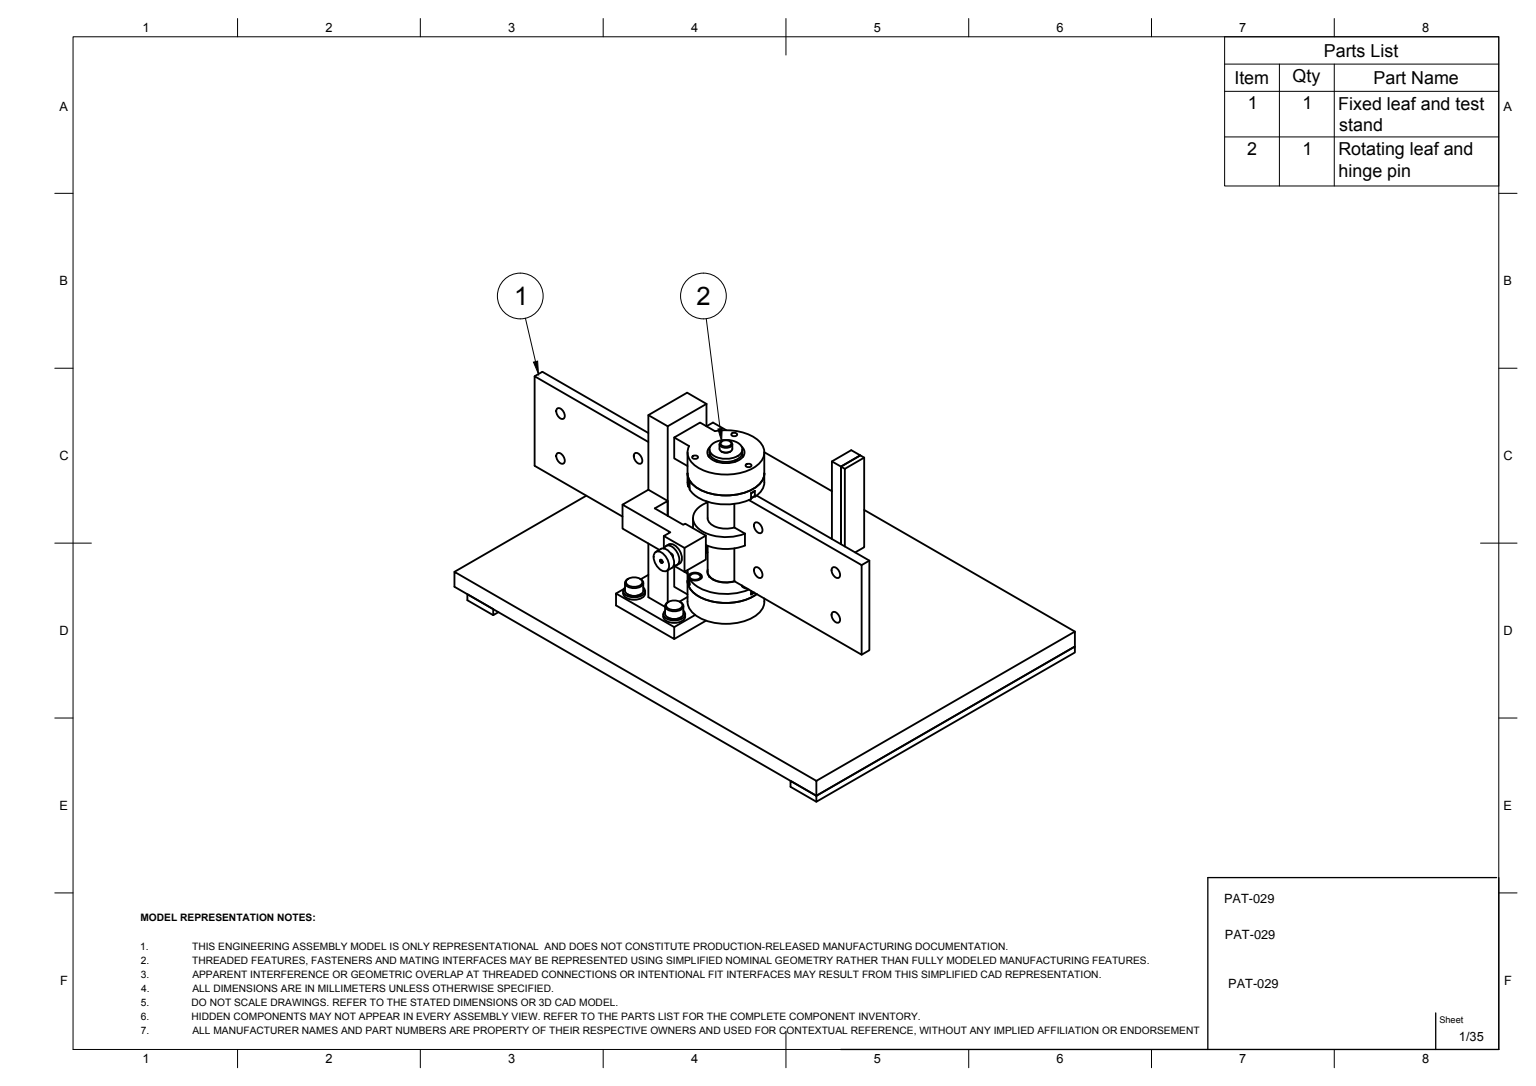
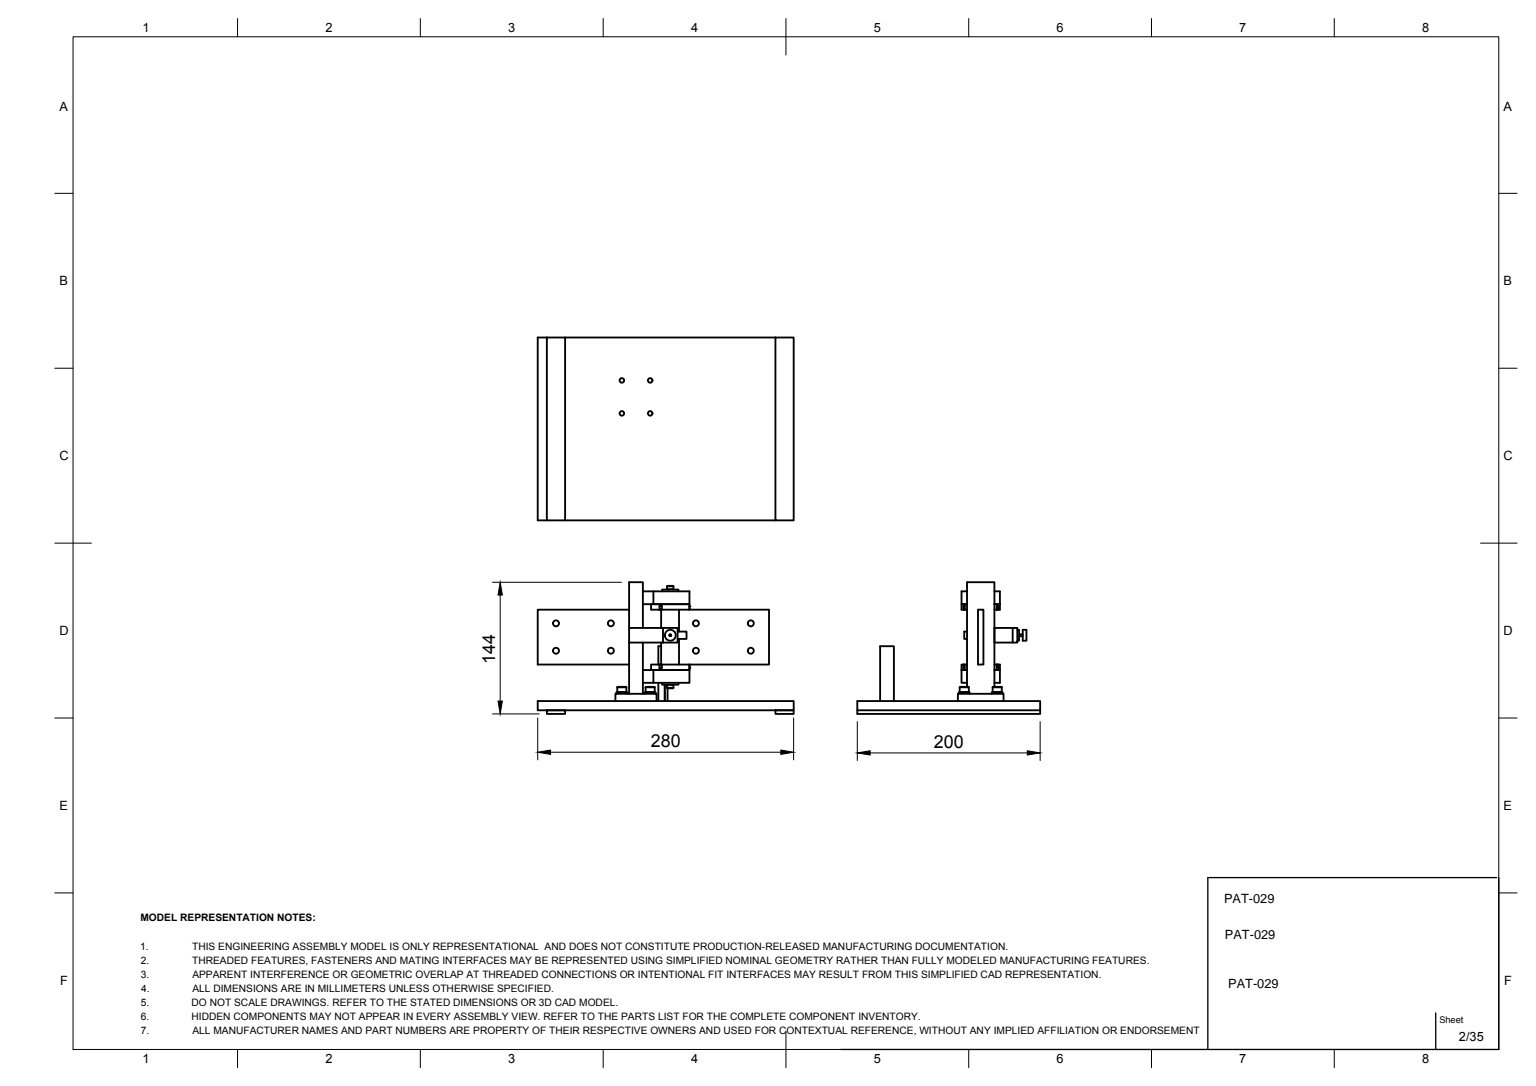
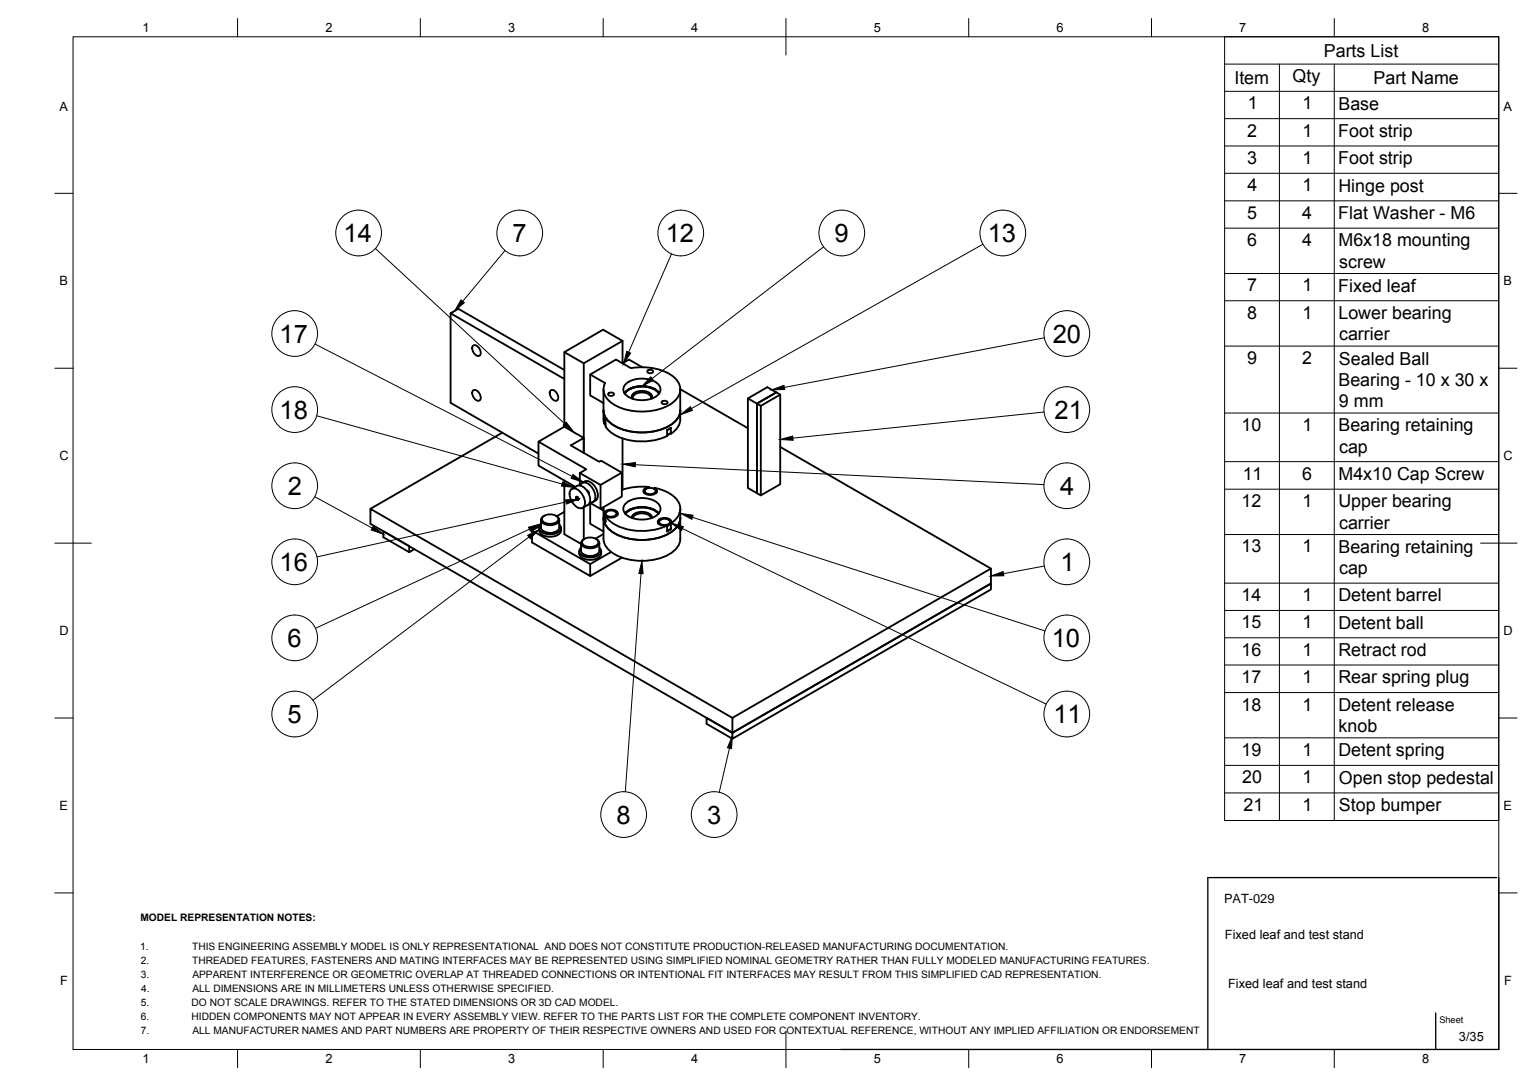
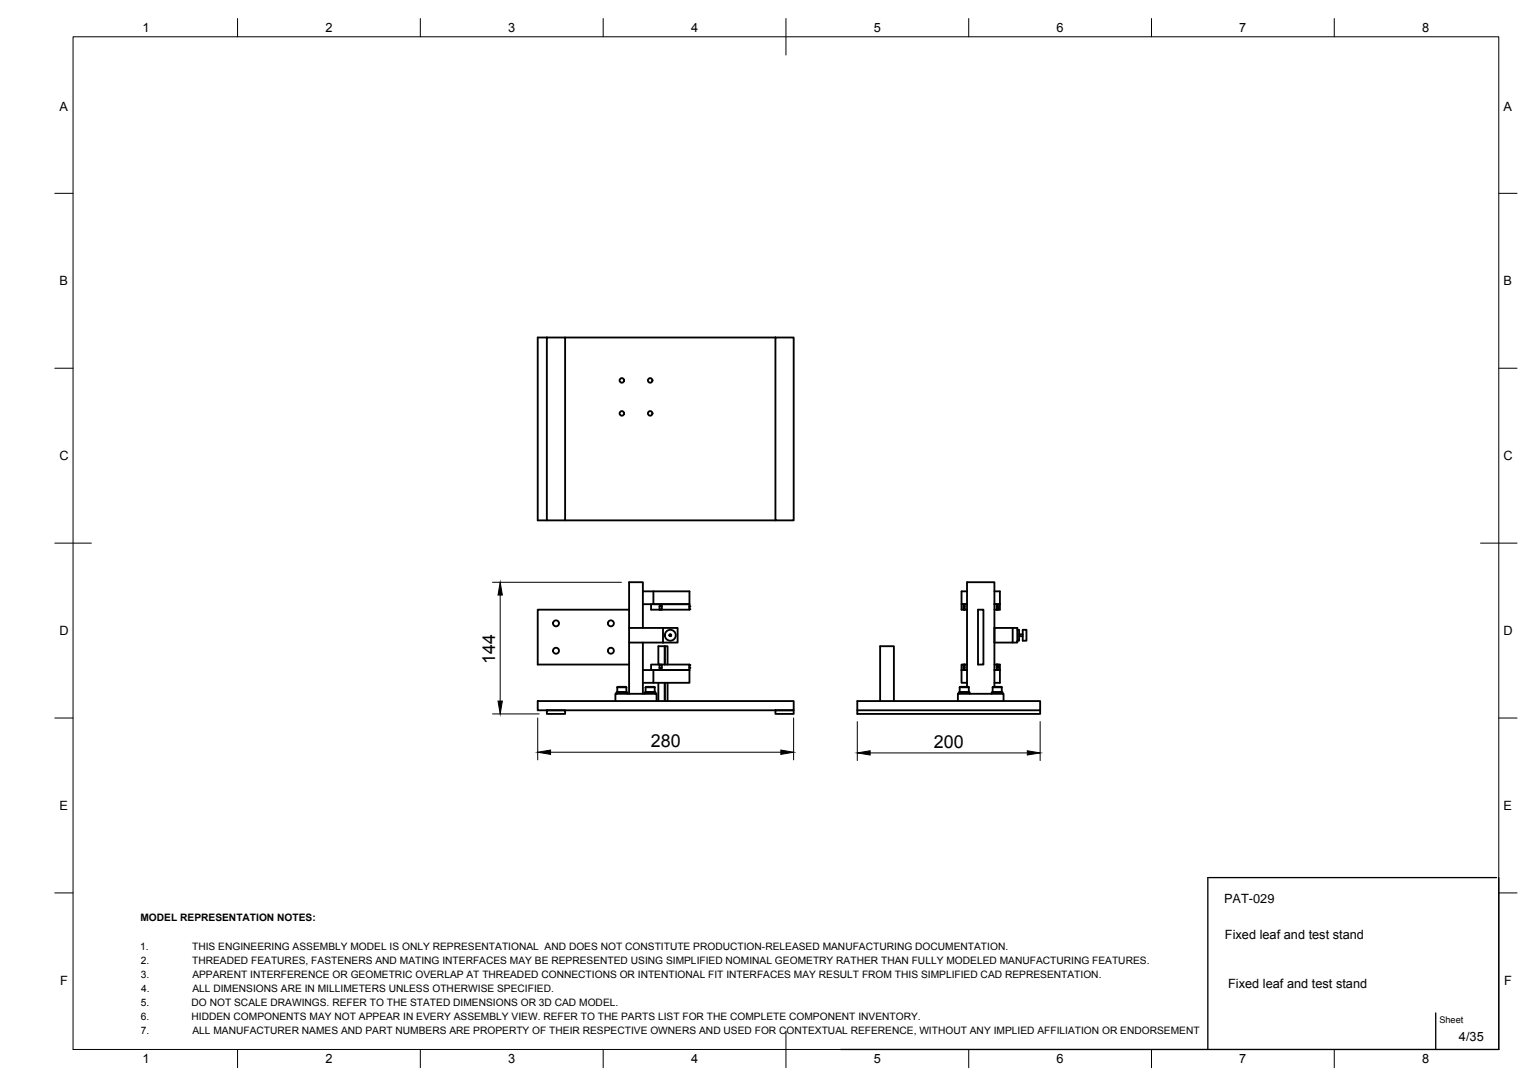
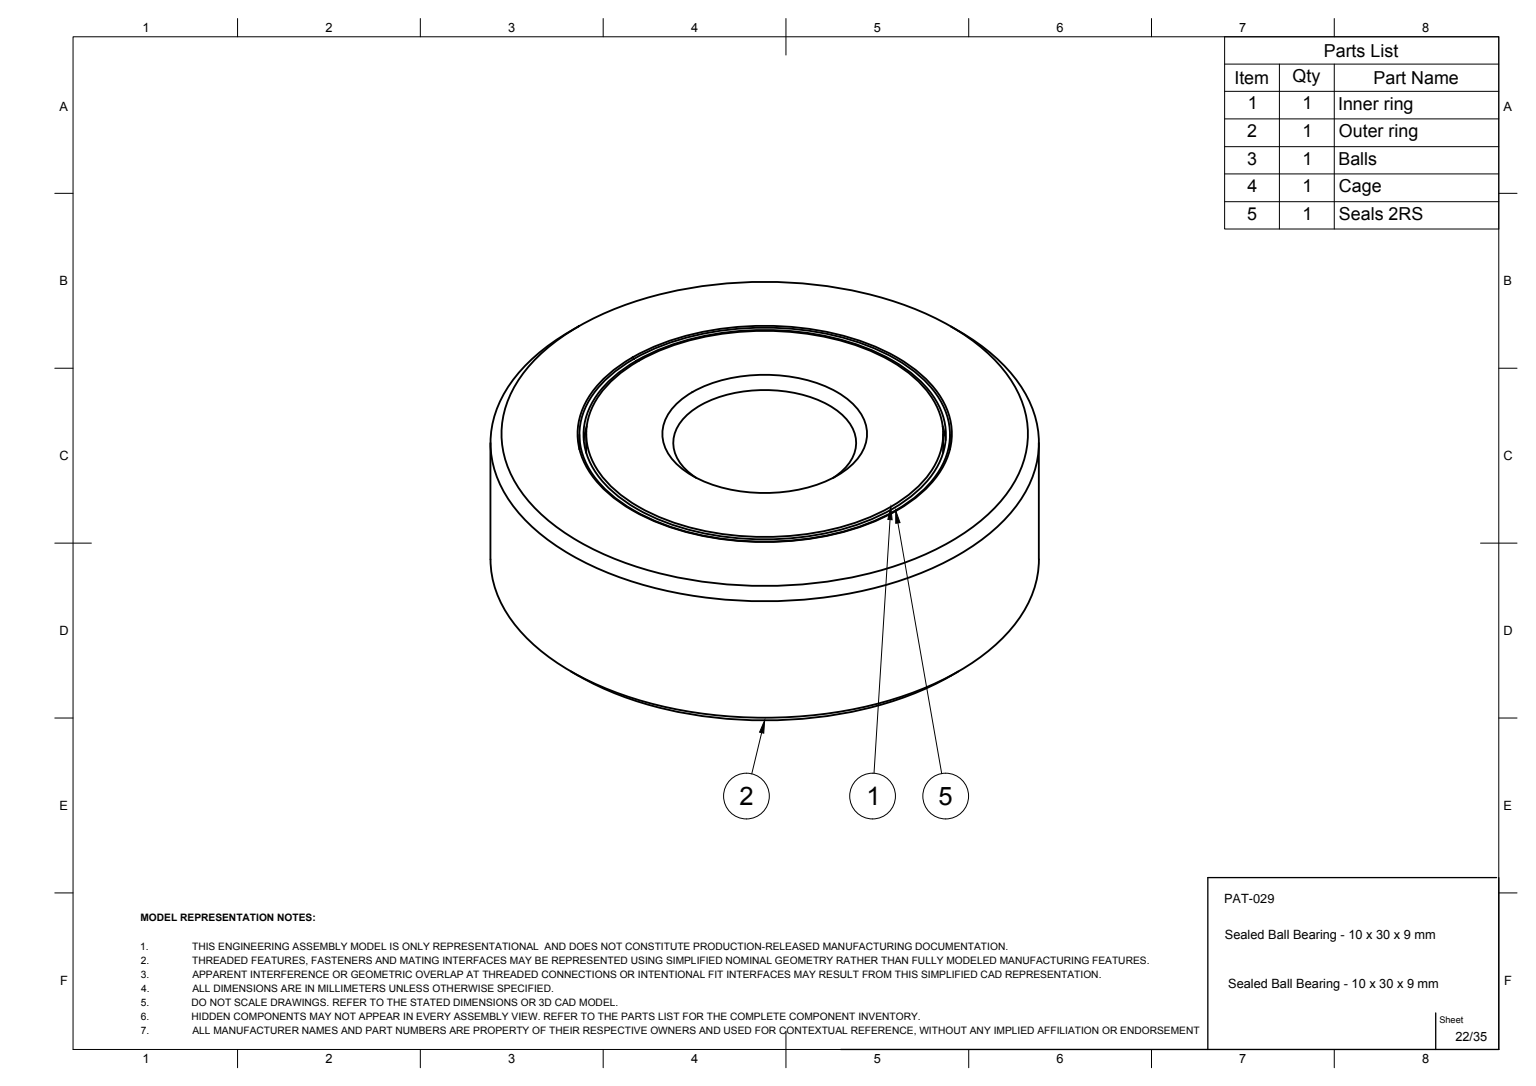
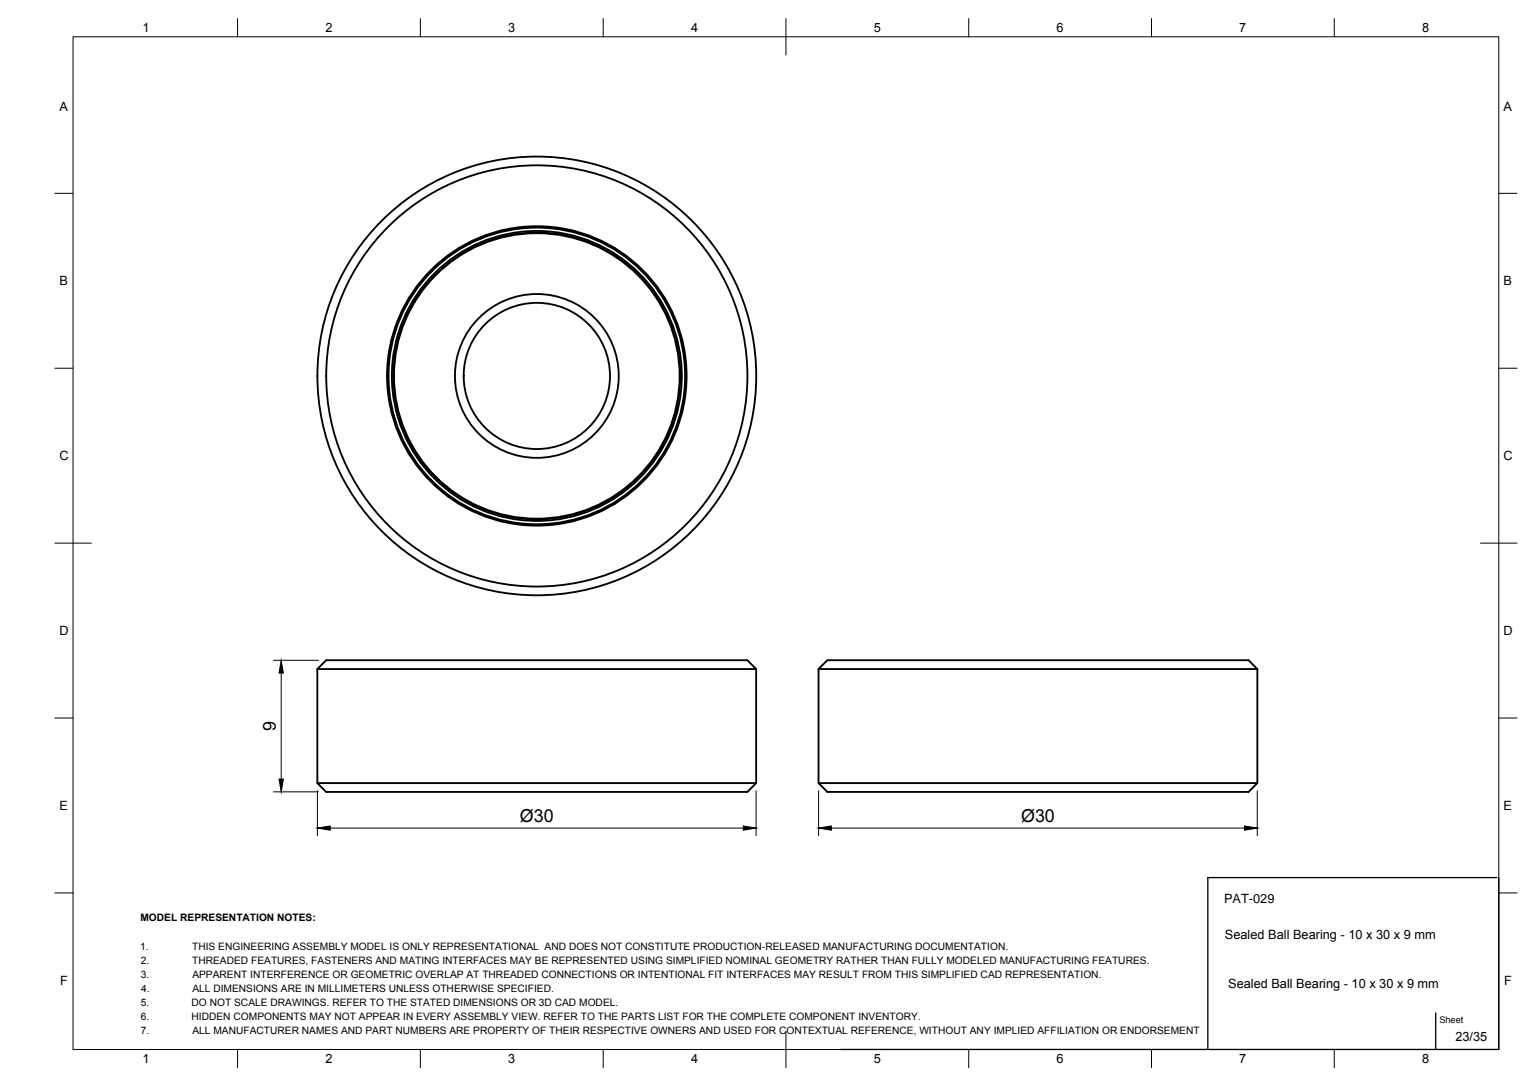
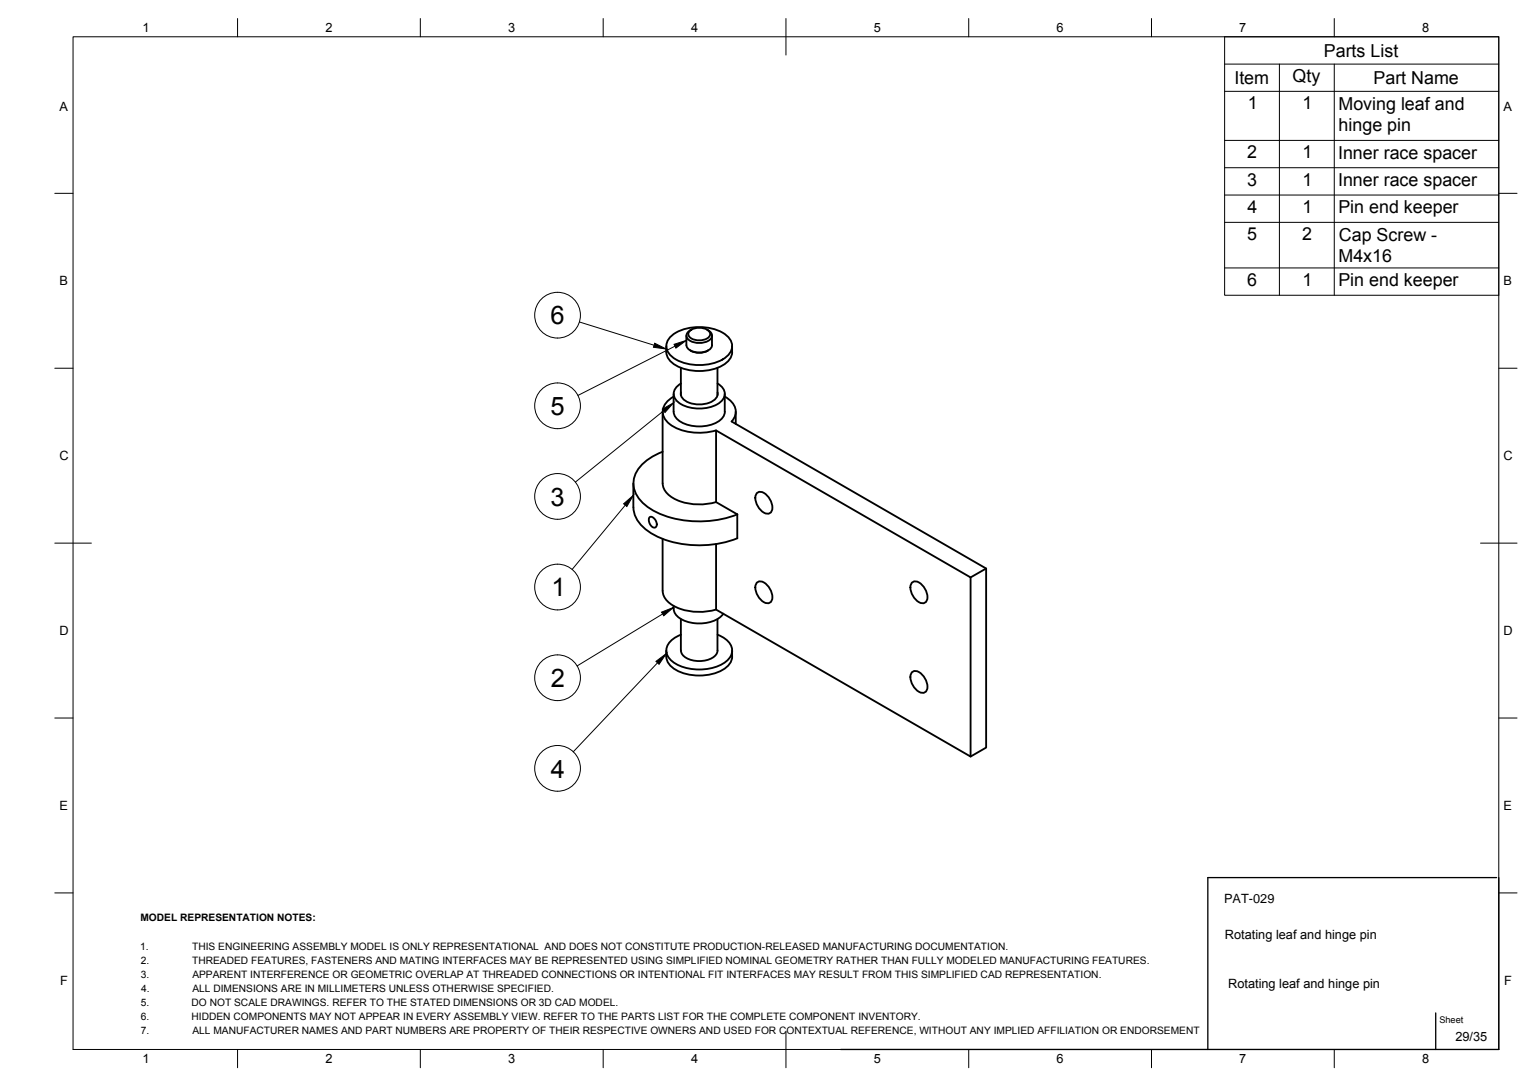
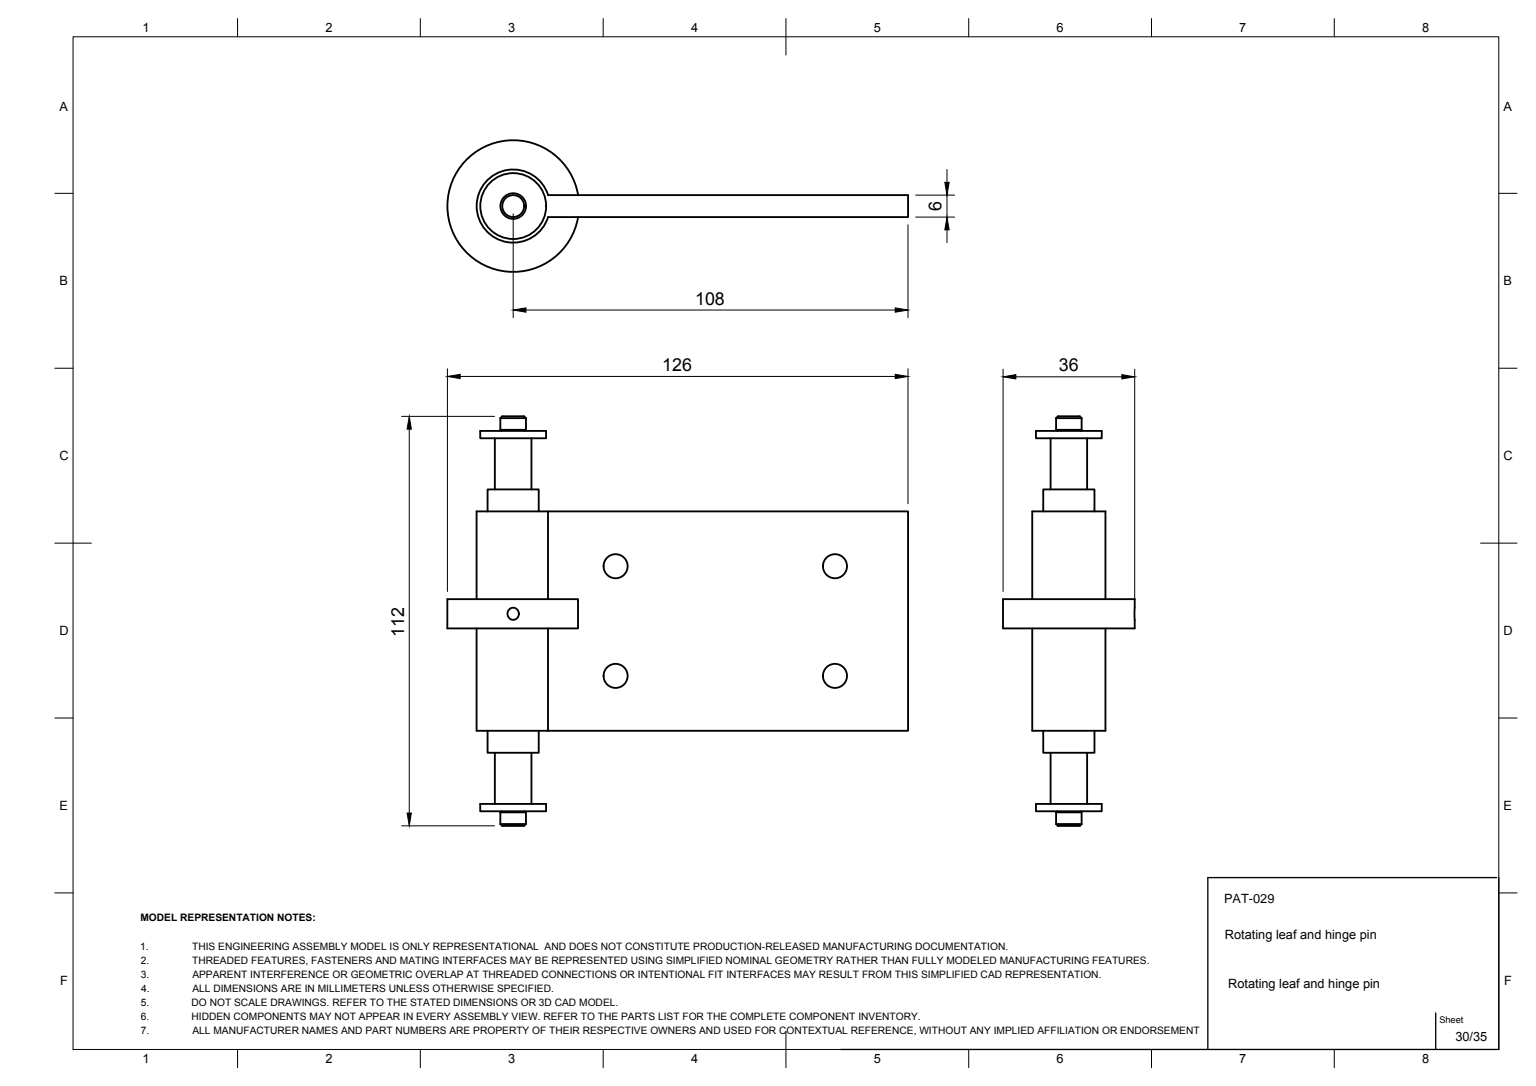
ISO-10303-21;
HEADER;
/* Generated by software containing ST-Developer
 * from STEP Tools, Inc. (www.steptools.com) 
 */

FILE_DESCRIPTION(
/* description */ ('Door-style hinge test fixture with detent'),
/* implementation_level */ '2;1');

FILE_NAME(
/* name */ 'PAT-029',
/* time_stamp */ '2026-10-28T03:24:57-07:00',
/* author */ (''),
/* organization */ (''),
/* preprocessor_version */ 'ST-DEVELOPER v20.2',
/* originating_system */ 'Autodesk Translation Framework v15.17.0.0',
/* authorisation */ '');

FILE_SCHEMA (('AUTOMOTIVE_DESIGN { 1 0 10303 214 3 1 1 }'));
ENDSEC;

DATA;
#10=MECHANICAL_DESIGN_GEOMETRIC_PRESENTATION_REPRESENTATION('',(#322,#323,
#324,#325,#326,#327,#328,#329,#330,#331,#332,#333,#334,#335,#336,#337,#338,
#339,#340,#341,#342,#343,#344,#345,#346,#347,#348,#349,#350,#351,#352,#353,
#354,#355,#356,#357,#358,#359,#360,#361),#9813);
#11=ITEM_DEFINED_TRANSFORMATION($,$,#5443,#5571);
#12=ITEM_DEFINED_TRANSFORMATION($,$,#5463,#5572);
#13=ITEM_DEFINED_TRANSFORMATION($,$,#5483,#5573);
#14=ITEM_DEFINED_TRANSFORMATION($,$,#5500,#5574);
#15=ITEM_DEFINED_TRANSFORMATION($,$,#5554,#5575);
#16=ITEM_DEFINED_TRANSFORMATION($,$,#5140,#5600);
#17=ITEM_DEFINED_TRANSFORMATION($,$,#5159,#5601);
#18=ITEM_DEFINED_TRANSFORMATION($,$,#5166,#5602);
#19=ITEM_DEFINED_TRANSFORMATION($,$,#5173,#5603);
#20=ITEM_DEFINED_TRANSFORMATION($,$,#5198,#5604);
#21=ITEM_DEFINED_TRANSFORMATION($,$,#5217,#5605);
#22=ITEM_DEFINED_TRANSFORMATION($,$,#5242,#5606);
#23=ITEM_DEFINED_TRANSFORMATION($,$,#5278,#5607);
#24=ITEM_DEFINED_TRANSFORMATION($,$,#5303,#5608);
#25=ITEM_DEFINED_TRANSFORMATION($,$,#5339,#5609);
#26=ITEM_DEFINED_TRANSFORMATION($,$,#5355,#5610);
#27=ITEM_DEFINED_TRANSFORMATION($,$,#5358,#5611);
#28=ITEM_DEFINED_TRANSFORMATION($,$,#5368,#5612);
#29=ITEM_DEFINED_TRANSFORMATION($,$,#5381,#5613);
#30=ITEM_DEFINED_TRANSFORMATION($,$,#5390,#5614);
#31=ITEM_DEFINED_TRANSFORMATION($,$,#5395,#5615);
#32=ITEM_DEFINED_TRANSFORMATION($,$,#5402,#5616);
#33=ITEM_DEFINED_TRANSFORMATION($,$,#5409,#5617);
#34=ITEM_DEFINED_TRANSFORMATION($,$,#5418,#5618);
#35=ITEM_DEFINED_TRANSFORMATION($,$,#5409,#5619);
#36=ITEM_DEFINED_TRANSFORMATION($,$,#5418,#5620);
#37=ITEM_DEFINED_TRANSFORMATION($,$,#5409,#5621);
#38=ITEM_DEFINED_TRANSFORMATION($,$,#5418,#5622);
#39=ITEM_DEFINED_TRANSFORMATION($,$,#5409,#5623);
#40=ITEM_DEFINED_TRANSFORMATION($,$,#5418,#5624);
#41=ITEM_DEFINED_TRANSFORMATION($,$,#5442,#5625);
#42=ITEM_DEFINED_TRANSFORMATION($,$,#5576,#5626);
#43=ITEM_DEFINED_TRANSFORMATION($,$,#5576,#5627);
#44=ITEM_DEFINED_TRANSFORMATION($,$,#5576,#5628);
#45=ITEM_DEFINED_TRANSFORMATION($,$,#5442,#5629);
#46=ITEM_DEFINED_TRANSFORMATION($,$,#5576,#5630);
#47=ITEM_DEFINED_TRANSFORMATION($,$,#5576,#5631);
#48=ITEM_DEFINED_TRANSFORMATION($,$,#5576,#5632);
#49=ITEM_DEFINED_TRANSFORMATION($,$,#5634,#5742);
#50=ITEM_DEFINED_TRANSFORMATION($,$,#5680,#5743);
#51=ITEM_DEFINED_TRANSFORMATION($,$,#5689,#5744);
#52=ITEM_DEFINED_TRANSFORMATION($,$,#5698,#5745);
#53=ITEM_DEFINED_TRANSFORMATION($,$,#5707,#5746);
#54=ITEM_DEFINED_TRANSFORMATION($,$,#5716,#5747);
#55=ITEM_DEFINED_TRANSFORMATION($,$,#5716,#5748);
#56=ITEM_DEFINED_TRANSFORMATION($,$,#5139,#5749);
#57=ITEM_DEFINED_TRANSFORMATION($,$,#5633,#5750);
#58=(
REPRESENTATION_RELATIONSHIP($,$,#9957,#9956)
REPRESENTATION_RELATIONSHIP_WITH_TRANSFORMATION(#11)
SHAPE_REPRESENTATION_RELATIONSHIP()
);
#59=(
REPRESENTATION_RELATIONSHIP($,$,#9958,#9956)
REPRESENTATION_RELATIONSHIP_WITH_TRANSFORMATION(#12)
SHAPE_REPRESENTATION_RELATIONSHIP()
);
#60=(
REPRESENTATION_RELATIONSHIP($,$,#9959,#9956)
REPRESENTATION_RELATIONSHIP_WITH_TRANSFORMATION(#13)
SHAPE_REPRESENTATION_RELATIONSHIP()
);
#61=(
REPRESENTATION_RELATIONSHIP($,$,#9960,#9956)
REPRESENTATION_RELATIONSHIP_WITH_TRANSFORMATION(#14)
SHAPE_REPRESENTATION_RELATIONSHIP()
);
#62=(
REPRESENTATION_RELATIONSHIP($,$,#9961,#9956)
REPRESENTATION_RELATIONSHIP_WITH_TRANSFORMATION(#15)
SHAPE_REPRESENTATION_RELATIONSHIP()
);
#63=(
REPRESENTATION_RELATIONSHIP($,$,#9937,#9936)
REPRESENTATION_RELATIONSHIP_WITH_TRANSFORMATION(#16)
SHAPE_REPRESENTATION_RELATIONSHIP()
);
#64=(
REPRESENTATION_RELATIONSHIP($,$,#9938,#9936)
REPRESENTATION_RELATIONSHIP_WITH_TRANSFORMATION(#17)
SHAPE_REPRESENTATION_RELATIONSHIP()
);
#65=(
REPRESENTATION_RELATIONSHIP($,$,#9939,#9936)
REPRESENTATION_RELATIONSHIP_WITH_TRANSFORMATION(#18)
SHAPE_REPRESENTATION_RELATIONSHIP()
);
#66=(
REPRESENTATION_RELATIONSHIP($,$,#9940,#9936)
REPRESENTATION_RELATIONSHIP_WITH_TRANSFORMATION(#19)
SHAPE_REPRESENTATION_RELATIONSHIP()
);
#67=(
REPRESENTATION_RELATIONSHIP($,$,#9941,#9936)
REPRESENTATION_RELATIONSHIP_WITH_TRANSFORMATION(#20)
SHAPE_REPRESENTATION_RELATIONSHIP()
);
#68=(
REPRESENTATION_RELATIONSHIP($,$,#9942,#9936)
REPRESENTATION_RELATIONSHIP_WITH_TRANSFORMATION(#21)
SHAPE_REPRESENTATION_RELATIONSHIP()
);
#69=(
REPRESENTATION_RELATIONSHIP($,$,#9943,#9936)
REPRESENTATION_RELATIONSHIP_WITH_TRANSFORMATION(#22)
SHAPE_REPRESENTATION_RELATIONSHIP()
);
#70=(
REPRESENTATION_RELATIONSHIP($,$,#9944,#9936)
REPRESENTATION_RELATIONSHIP_WITH_TRANSFORMATION(#23)
SHAPE_REPRESENTATION_RELATIONSHIP()
);
#71=(
REPRESENTATION_RELATIONSHIP($,$,#9945,#9936)
REPRESENTATION_RELATIONSHIP_WITH_TRANSFORMATION(#24)
SHAPE_REPRESENTATION_RELATIONSHIP()
);
#72=(
REPRESENTATION_RELATIONSHIP($,$,#9946,#9936)
REPRESENTATION_RELATIONSHIP_WITH_TRANSFORMATION(#25)
SHAPE_REPRESENTATION_RELATIONSHIP()
);
#73=(
REPRESENTATION_RELATIONSHIP($,$,#9947,#9936)
REPRESENTATION_RELATIONSHIP_WITH_TRANSFORMATION(#26)
SHAPE_REPRESENTATION_RELATIONSHIP()
);
#74=(
REPRESENTATION_RELATIONSHIP($,$,#9948,#9936)
REPRESENTATION_RELATIONSHIP_WITH_TRANSFORMATION(#27)
SHAPE_REPRESENTATION_RELATIONSHIP()
);
#75=(
REPRESENTATION_RELATIONSHIP($,$,#9949,#9936)
REPRESENTATION_RELATIONSHIP_WITH_TRANSFORMATION(#28)
SHAPE_REPRESENTATION_RELATIONSHIP()
);
#76=(
REPRESENTATION_RELATIONSHIP($,$,#9950,#9936)
REPRESENTATION_RELATIONSHIP_WITH_TRANSFORMATION(#29)
SHAPE_REPRESENTATION_RELATIONSHIP()
);
#77=(
REPRESENTATION_RELATIONSHIP($,$,#9951,#9936)
REPRESENTATION_RELATIONSHIP_WITH_TRANSFORMATION(#30)
SHAPE_REPRESENTATION_RELATIONSHIP()
);
#78=(
REPRESENTATION_RELATIONSHIP($,$,#9952,#9936)
REPRESENTATION_RELATIONSHIP_WITH_TRANSFORMATION(#31)
SHAPE_REPRESENTATION_RELATIONSHIP()
);
#79=(
REPRESENTATION_RELATIONSHIP($,$,#9953,#9936)
REPRESENTATION_RELATIONSHIP_WITH_TRANSFORMATION(#32)
SHAPE_REPRESENTATION_RELATIONSHIP()
);
#80=(
REPRESENTATION_RELATIONSHIP($,$,#9954,#9936)
REPRESENTATION_RELATIONSHIP_WITH_TRANSFORMATION(#33)
SHAPE_REPRESENTATION_RELATIONSHIP()
);
#81=(
REPRESENTATION_RELATIONSHIP($,$,#9955,#9936)
REPRESENTATION_RELATIONSHIP_WITH_TRANSFORMATION(#34)
SHAPE_REPRESENTATION_RELATIONSHIP()
);
#82=(
REPRESENTATION_RELATIONSHIP($,$,#9954,#9936)
REPRESENTATION_RELATIONSHIP_WITH_TRANSFORMATION(#35)
SHAPE_REPRESENTATION_RELATIONSHIP()
);
#83=(
REPRESENTATION_RELATIONSHIP($,$,#9955,#9936)
REPRESENTATION_RELATIONSHIP_WITH_TRANSFORMATION(#36)
SHAPE_REPRESENTATION_RELATIONSHIP()
);
#84=(
REPRESENTATION_RELATIONSHIP($,$,#9954,#9936)
REPRESENTATION_RELATIONSHIP_WITH_TRANSFORMATION(#37)
SHAPE_REPRESENTATION_RELATIONSHIP()
);
#85=(
REPRESENTATION_RELATIONSHIP($,$,#9955,#9936)
REPRESENTATION_RELATIONSHIP_WITH_TRANSFORMATION(#38)
SHAPE_REPRESENTATION_RELATIONSHIP()
);
#86=(
REPRESENTATION_RELATIONSHIP($,$,#9954,#9936)
REPRESENTATION_RELATIONSHIP_WITH_TRANSFORMATION(#39)
SHAPE_REPRESENTATION_RELATIONSHIP()
);
#87=(
REPRESENTATION_RELATIONSHIP($,$,#9955,#9936)
REPRESENTATION_RELATIONSHIP_WITH_TRANSFORMATION(#40)
SHAPE_REPRESENTATION_RELATIONSHIP()
);
#88=(
REPRESENTATION_RELATIONSHIP($,$,#9956,#9936)
REPRESENTATION_RELATIONSHIP_WITH_TRANSFORMATION(#41)
SHAPE_REPRESENTATION_RELATIONSHIP()
);
#89=(
REPRESENTATION_RELATIONSHIP($,$,#9962,#9936)
REPRESENTATION_RELATIONSHIP_WITH_TRANSFORMATION(#42)
SHAPE_REPRESENTATION_RELATIONSHIP()
);
#90=(
REPRESENTATION_RELATIONSHIP($,$,#9962,#9936)
REPRESENTATION_RELATIONSHIP_WITH_TRANSFORMATION(#43)
SHAPE_REPRESENTATION_RELATIONSHIP()
);
#91=(
REPRESENTATION_RELATIONSHIP($,$,#9962,#9936)
REPRESENTATION_RELATIONSHIP_WITH_TRANSFORMATION(#44)
SHAPE_REPRESENTATION_RELATIONSHIP()
);
#92=(
REPRESENTATION_RELATIONSHIP($,$,#9956,#9936)
REPRESENTATION_RELATIONSHIP_WITH_TRANSFORMATION(#45)
SHAPE_REPRESENTATION_RELATIONSHIP()
);
#93=(
REPRESENTATION_RELATIONSHIP($,$,#9962,#9936)
REPRESENTATION_RELATIONSHIP_WITH_TRANSFORMATION(#46)
SHAPE_REPRESENTATION_RELATIONSHIP()
);
#94=(
REPRESENTATION_RELATIONSHIP($,$,#9962,#9936)
REPRESENTATION_RELATIONSHIP_WITH_TRANSFORMATION(#47)
SHAPE_REPRESENTATION_RELATIONSHIP()
);
#95=(
REPRESENTATION_RELATIONSHIP($,$,#9962,#9936)
REPRESENTATION_RELATIONSHIP_WITH_TRANSFORMATION(#48)
SHAPE_REPRESENTATION_RELATIONSHIP()
);
#96=(
REPRESENTATION_RELATIONSHIP($,$,#9964,#9963)
REPRESENTATION_RELATIONSHIP_WITH_TRANSFORMATION(#49)
SHAPE_REPRESENTATION_RELATIONSHIP()
);
#97=(
REPRESENTATION_RELATIONSHIP($,$,#9965,#9963)
REPRESENTATION_RELATIONSHIP_WITH_TRANSFORMATION(#50)
SHAPE_REPRESENTATION_RELATIONSHIP()
);
#98=(
REPRESENTATION_RELATIONSHIP($,$,#9966,#9963)
REPRESENTATION_RELATIONSHIP_WITH_TRANSFORMATION(#51)
SHAPE_REPRESENTATION_RELATIONSHIP()
);
#99=(
REPRESENTATION_RELATIONSHIP($,$,#9967,#9963)
REPRESENTATION_RELATIONSHIP_WITH_TRANSFORMATION(#52)
SHAPE_REPRESENTATION_RELATIONSHIP()
);
#100=(
REPRESENTATION_RELATIONSHIP($,$,#9968,#9963)
REPRESENTATION_RELATIONSHIP_WITH_TRANSFORMATION(#53)
SHAPE_REPRESENTATION_RELATIONSHIP()
);
#101=(
REPRESENTATION_RELATIONSHIP($,$,#9969,#9963)
REPRESENTATION_RELATIONSHIP_WITH_TRANSFORMATION(#54)
SHAPE_REPRESENTATION_RELATIONSHIP()
);
#102=(
REPRESENTATION_RELATIONSHIP($,$,#9969,#9963)
REPRESENTATION_RELATIONSHIP_WITH_TRANSFORMATION(#55)
SHAPE_REPRESENTATION_RELATIONSHIP()
);
#103=(
REPRESENTATION_RELATIONSHIP($,$,#9936,#9935)
REPRESENTATION_RELATIONSHIP_WITH_TRANSFORMATION(#56)
SHAPE_REPRESENTATION_RELATIONSHIP()
);
#104=(
REPRESENTATION_RELATIONSHIP($,$,#9963,#9935)
REPRESENTATION_RELATIONSHIP_WITH_TRANSFORMATION(#57)
SHAPE_REPRESENTATION_RELATIONSHIP()
);
#105=CONTEXT_DEPENDENT_SHAPE_REPRESENTATION(#58,#9880);
#106=CONTEXT_DEPENDENT_SHAPE_REPRESENTATION(#59,#9881);
#107=CONTEXT_DEPENDENT_SHAPE_REPRESENTATION(#60,#9882);
#108=CONTEXT_DEPENDENT_SHAPE_REPRESENTATION(#61,#9883);
#109=CONTEXT_DEPENDENT_SHAPE_REPRESENTATION(#62,#9884);
#110=CONTEXT_DEPENDENT_SHAPE_REPRESENTATION(#63,#9886);
#111=CONTEXT_DEPENDENT_SHAPE_REPRESENTATION(#64,#9887);
#112=CONTEXT_DEPENDENT_SHAPE_REPRESENTATION(#65,#9888);
#113=CONTEXT_DEPENDENT_SHAPE_REPRESENTATION(#66,#9889);
#114=CONTEXT_DEPENDENT_SHAPE_REPRESENTATION(#67,#9890);
#115=CONTEXT_DEPENDENT_SHAPE_REPRESENTATION(#68,#9891);
#116=CONTEXT_DEPENDENT_SHAPE_REPRESENTATION(#69,#9892);
#117=CONTEXT_DEPENDENT_SHAPE_REPRESENTATION(#70,#9893);
#118=CONTEXT_DEPENDENT_SHAPE_REPRESENTATION(#71,#9894);
#119=CONTEXT_DEPENDENT_SHAPE_REPRESENTATION(#72,#9895);
#120=CONTEXT_DEPENDENT_SHAPE_REPRESENTATION(#73,#9896);
#121=CONTEXT_DEPENDENT_SHAPE_REPRESENTATION(#74,#9897);
#122=CONTEXT_DEPENDENT_SHAPE_REPRESENTATION(#75,#9898);
#123=CONTEXT_DEPENDENT_SHAPE_REPRESENTATION(#76,#9899);
#124=CONTEXT_DEPENDENT_SHAPE_REPRESENTATION(#77,#9900);
#125=CONTEXT_DEPENDENT_SHAPE_REPRESENTATION(#78,#9901);
#126=CONTEXT_DEPENDENT_SHAPE_REPRESENTATION(#79,#9902);
#127=CONTEXT_DEPENDENT_SHAPE_REPRESENTATION(#80,#9903);
#128=CONTEXT_DEPENDENT_SHAPE_REPRESENTATION(#81,#9904);
#129=CONTEXT_DEPENDENT_SHAPE_REPRESENTATION(#82,#9905);
#130=CONTEXT_DEPENDENT_SHAPE_REPRESENTATION(#83,#9906);
#131=CONTEXT_DEPENDENT_SHAPE_REPRESENTATION(#84,#9907);
#132=CONTEXT_DEPENDENT_SHAPE_REPRESENTATION(#85,#9908);
#133=CONTEXT_DEPENDENT_SHAPE_REPRESENTATION(#86,#9909);
#134=CONTEXT_DEPENDENT_SHAPE_REPRESENTATION(#87,#9910);
#135=CONTEXT_DEPENDENT_SHAPE_REPRESENTATION(#88,#9911);
#136=CONTEXT_DEPENDENT_SHAPE_REPRESENTATION(#89,#9912);
#137=CONTEXT_DEPENDENT_SHAPE_REPRESENTATION(#90,#9913);
#138=CONTEXT_DEPENDENT_SHAPE_REPRESENTATION(#91,#9914);
#139=CONTEXT_DEPENDENT_SHAPE_REPRESENTATION(#92,#9915);
#140=CONTEXT_DEPENDENT_SHAPE_REPRESENTATION(#93,#9916);
#141=CONTEXT_DEPENDENT_SHAPE_REPRESENTATION(#94,#9917);
#142=CONTEXT_DEPENDENT_SHAPE_REPRESENTATION(#95,#9918);
#143=CONTEXT_DEPENDENT_SHAPE_REPRESENTATION(#96,#9926);
#144=CONTEXT_DEPENDENT_SHAPE_REPRESENTATION(#97,#9927);
#145=CONTEXT_DEPENDENT_SHAPE_REPRESENTATION(#98,#9928);
#146=CONTEXT_DEPENDENT_SHAPE_REPRESENTATION(#99,#9929);
#147=CONTEXT_DEPENDENT_SHAPE_REPRESENTATION(#100,#9930);
#148=CONTEXT_DEPENDENT_SHAPE_REPRESENTATION(#101,#9931);
#149=CONTEXT_DEPENDENT_SHAPE_REPRESENTATION(#102,#9932);
#150=CONTEXT_DEPENDENT_SHAPE_REPRESENTATION(#103,#9933);
#151=CONTEXT_DEPENDENT_SHAPE_REPRESENTATION(#104,#9934);
#152=NEXT_ASSEMBLY_USAGE_OCCURRENCE('Inner ring:1','Inner ring:1',
'Inner ring:1',#9992,#9993,'Inner ring:1');
#153=NEXT_ASSEMBLY_USAGE_OCCURRENCE('Outer ring:1','Outer ring:1',
'Outer ring:1',#9992,#9994,'Outer ring:1');
#154=NEXT_ASSEMBLY_USAGE_OCCURRENCE('Balls:1','Balls:1','Balls:1',#9992,
#9995,'Balls:1');
#155=NEXT_ASSEMBLY_USAGE_OCCURRENCE('Cage:1','Cage:1','Cage:1',#9992,#9996,
'Cage:1');
#156=NEXT_ASSEMBLY_USAGE_OCCURRENCE('Seals 2RS:1','Seals 2RS:1',
'Seals 2RS:1',#9992,#9997,'Seals 2RS:1');
#157=NEXT_ASSEMBLY_USAGE_OCCURRENCE('Base:1','Base:1','Base:1',#9972,#9973,
'Base:1');
#158=NEXT_ASSEMBLY_USAGE_OCCURRENCE('Foot strip:1','Foot strip:1',
'Foot strip:1',#9972,#9974,'Foot strip:1');
#159=NEXT_ASSEMBLY_USAGE_OCCURRENCE('Foot strip (1):1',
'Foot strip (1):1','Foot strip (1):1',#9972,#9975,'Foot strip (1):1');
#160=NEXT_ASSEMBLY_USAGE_OCCURRENCE('Hinge post:1','Hinge post:1',
'Hinge post:1',#9972,#9976,'Hinge post:1');
#161=NEXT_ASSEMBLY_USAGE_OCCURRENCE('Fixed leaf:1','Fixed leaf:1',
'Fixed leaf:1',#9972,#9977,'Fixed leaf:1');
#162=NEXT_ASSEMBLY_USAGE_OCCURRENCE('Lower bearing carrier:1',
'Lower bearing carrier:1','Lower bearing carrier:1',#9972,#9978,
'Lower bearing carrier:1');
#163=NEXT_ASSEMBLY_USAGE_OCCURRENCE('Bearing retaining cap:1',
'Bearing retaining cap:1','Bearing retaining cap:1',#9972,#9979,
'Bearing retaining cap:1');
#164=NEXT_ASSEMBLY_USAGE_OCCURRENCE('Upper bearing carrier:1',
'Upper bearing carrier:1','Upper bearing carrier:1',#9972,#9980,
'Upper bearing carrier:1');
#165=NEXT_ASSEMBLY_USAGE_OCCURRENCE('Bearing retaining cap (1):1',
'Bearing retaining cap (1):1','Bearing retaining cap (1):1',#9972,#9981,
'Bearing retaining cap (1):1');
#166=NEXT_ASSEMBLY_USAGE_OCCURRENCE('Detent barrel:1','Detent barrel:1',
'Detent barrel:1',#9972,#9982,'Detent barrel:1');
#167=NEXT_ASSEMBLY_USAGE_OCCURRENCE('Detent ball:1','Detent ball:1',
'Detent ball:1',#9972,#9983,'Detent ball:1');
#168=NEXT_ASSEMBLY_USAGE_OCCURRENCE('Retract rod:1','Retract rod:1',
'Retract rod:1',#9972,#9984,'Retract rod:1');
#169=NEXT_ASSEMBLY_USAGE_OCCURRENCE('Rear spring plug:1',
'Rear spring plug:1','Rear spring plug:1',#9972,#9985,
'Rear spring plug:1');
#170=NEXT_ASSEMBLY_USAGE_OCCURRENCE('Detent release knob:1',
'Detent release knob:1','Detent release knob:1',#9972,#9986,
'Detent release knob:1');
#171=NEXT_ASSEMBLY_USAGE_OCCURRENCE('Detent spring:1','Detent spring:1',
'Detent spring:1',#9972,#9987,'Detent spring:1');
#172=NEXT_ASSEMBLY_USAGE_OCCURRENCE('Open stop pedestal:1',
'Open stop pedestal:1','Open stop pedestal:1',#9972,#9988,
'Open stop pedestal:1');
#173=NEXT_ASSEMBLY_USAGE_OCCURRENCE('Stop bumper:1','Stop bumper:1',
'Stop bumper:1',#9972,#9989,'Stop bumper:1');
#174=NEXT_ASSEMBLY_USAGE_OCCURRENCE('Flat Washer - M6:2',
'Flat Washer - M6:2','Flat Washer - M6:2',#9972,#9990,
'Flat Washer - M6:2');
#175=NEXT_ASSEMBLY_USAGE_OCCURRENCE('M6x18 mounting screw:2',
'M6x18 mounting screw:2','M6x18 mounting screw:2',#9972,#9991,
'M6x18 mounting screw:2');
#176=NEXT_ASSEMBLY_USAGE_OCCURRENCE('Flat Washer - M6:3',
'Flat Washer - M6:3','Flat Washer - M6:3',#9972,#9990,
'Flat Washer - M6:3');
#177=NEXT_ASSEMBLY_USAGE_OCCURRENCE('M6x18 mounting screw:3',
'M6x18 mounting screw:3','M6x18 mounting screw:3',#9972,#9991,
'M6x18 mounting screw:3');
#178=NEXT_ASSEMBLY_USAGE_OCCURRENCE('Flat Washer - M6:4',
'Flat Washer - M6:4','Flat Washer - M6:4',#9972,#9990,
'Flat Washer - M6:4');
#179=NEXT_ASSEMBLY_USAGE_OCCURRENCE('M6x18 mounting screw:4',
'M6x18 mounting screw:4','M6x18 mounting screw:4',#9972,#9991,
'M6x18 mounting screw:4');
#180=NEXT_ASSEMBLY_USAGE_OCCURRENCE('Flat Washer - M6:5',
'Flat Washer - M6:5','Flat Washer - M6:5',#9972,#9990,
'Flat Washer - M6:5');
#181=NEXT_ASSEMBLY_USAGE_OCCURRENCE('M6x18 mounting screw:5',
'M6x18 mounting screw:5','M6x18 mounting screw:5',#9972,#9991,
'M6x18 mounting screw:5');
#182=NEXT_ASSEMBLY_USAGE_OCCURRENCE(
'Sealed Ball Bearing - 10 x 30 x 9 mm:2',
'Sealed Ball Bearing - 10 x 30 x 9 mm:2',
'Sealed Ball Bearing - 10 x 30 x 9 mm:2',#9972,#9992,
'Sealed Ball Bearing - 10 x 30 x 9 mm:2');
#183=NEXT_ASSEMBLY_USAGE_OCCURRENCE('M4x10 Cap Screw:2',
'M4x10 Cap Screw:2','M4x10 Cap Screw:2',#9972,#9998,'M4x10 Cap Screw:2');
#184=NEXT_ASSEMBLY_USAGE_OCCURRENCE('M4x10 Cap Screw:3',
'M4x10 Cap Screw:3','M4x10 Cap Screw:3',#9972,#9998,'M4x10 Cap Screw:3');
#185=NEXT_ASSEMBLY_USAGE_OCCURRENCE('M4x10 Cap Screw:4',
'M4x10 Cap Screw:4','M4x10 Cap Screw:4',#9972,#9998,'M4x10 Cap Screw:4');
#186=NEXT_ASSEMBLY_USAGE_OCCURRENCE(
'Sealed Ball Bearing - 10 x 30 x 9 mm:3',
'Sealed Ball Bearing - 10 x 30 x 9 mm:3',
'Sealed Ball Bearing - 10 x 30 x 9 mm:3',#9972,#9992,
'Sealed Ball Bearing - 10 x 30 x 9 mm:3');
#187=NEXT_ASSEMBLY_USAGE_OCCURRENCE('M4x10 Cap Screw:5',
'M4x10 Cap Screw:5','M4x10 Cap Screw:5',#9972,#9998,'M4x10 Cap Screw:5');
#188=NEXT_ASSEMBLY_USAGE_OCCURRENCE('M4x10 Cap Screw:6',
'M4x10 Cap Screw:6','M4x10 Cap Screw:6',#9972,#9998,'M4x10 Cap Screw:6');
#189=NEXT_ASSEMBLY_USAGE_OCCURRENCE('M4x10 Cap Screw:7',
'M4x10 Cap Screw:7','M4x10 Cap Screw:7',#9972,#9998,'M4x10 Cap Screw:7');
#190=NEXT_ASSEMBLY_USAGE_OCCURRENCE('Moving leaf and hinge pin:1',
'Moving leaf and hinge pin:1','Moving leaf and hinge pin:1',#9999,#10000,
'Moving leaf and hinge pin:1');
#191=NEXT_ASSEMBLY_USAGE_OCCURRENCE('Inner race spacer:1',
'Inner race spacer:1','Inner race spacer:1',#9999,#10001,
'Inner race spacer:1');
#192=NEXT_ASSEMBLY_USAGE_OCCURRENCE('Inner race spacer (1):1',
'Inner race spacer (1):1','Inner race spacer (1):1',#9999,#10002,
'Inner race spacer (1):1');
#193=NEXT_ASSEMBLY_USAGE_OCCURRENCE('Pin end keeper:1',
'Pin end keeper:1','Pin end keeper:1',#9999,#10003,'Pin end keeper:1');
#194=NEXT_ASSEMBLY_USAGE_OCCURRENCE('Pin end keeper (1):1',
'Pin end keeper (1):1','Pin end keeper (1):1',#9999,#10004,
'Pin end keeper (1):1');
#195=NEXT_ASSEMBLY_USAGE_OCCURRENCE('Cap Screw - M4x16:2',
'Cap Screw - M4x16:2','Cap Screw - M4x16:2',#9999,#10005,
'Cap Screw - M4x16:2');
#196=NEXT_ASSEMBLY_USAGE_OCCURRENCE('Cap Screw - M4x16:3',
'Cap Screw - M4x16:3','Cap Screw - M4x16:3',#9999,#10005,
'Cap Screw - M4x16:3');
#197=NEXT_ASSEMBLY_USAGE_OCCURRENCE('Fixed leaf and test stand:1',
'Fixed leaf and test stand:1','Fixed leaf and test stand:1',#9971,#9972,
'Fixed leaf and test stand:1');
#198=NEXT_ASSEMBLY_USAGE_OCCURRENCE('Rotating leaf and hinge pin:1',
'Rotating leaf and hinge pin:1','Rotating leaf and hinge pin:1',#9971,#9999,
'Rotating leaf and hinge pin:1');
#199=TOROIDAL_SURFACE('',#5444,1.,0.247676);
#200=TOROIDAL_SURFACE('',#5464,1.,0.247676);
#201=CONICAL_SURFACE('',#5431,0.475,0.785398163397449);
#202=CONICAL_SURFACE('',#5435,0.485,0.785398163397448);
#203=CONICAL_SURFACE('',#5439,0.31,0.463647609000806);
#204=CONICAL_SURFACE('',#5455,0.53,0.785398163397448);
#205=CONICAL_SURFACE('',#5462,0.53,0.785398163397448);
#206=CONICAL_SURFACE('',#5475,1.47,0.785398163397449);
#207=CONICAL_SURFACE('',#5479,1.47,0.785398163397449);
#208=CONICAL_SURFACE('',#5589,0.325,0.785398163397448);
#209=CONICAL_SURFACE('',#5593,0.335,0.785398163397448);
#210=CONICAL_SURFACE('',#5597,0.21,0.463647609000806);
#211=CONICAL_SURFACE('',#5719,0.325,0.785398163397448);
#212=CONICAL_SURFACE('',#5723,0.335,0.785398163397448);
#213=CONICAL_SURFACE('',#5727,0.21,0.463647609000806);
#214=CONICAL_SURFACE('',#5731,0.18,0.785398163397448);
#215=ORIENTED_CLOSED_SHELL('',*,#4772,.F.);
#216=ORIENTED_CLOSED_SHELL('',*,#4787,.F.);
#217=ORIENTED_CLOSED_SHELL('',*,#4795,.F.);
#218=BREP_WITH_VOIDS('Body1',#4773,(#215));
#219=BREP_WITH_VOIDS('Body1',#4788,(#216));
#220=BREP_WITH_VOIDS('Body1',#4794,(#217));
#221=B_SPLINE_CURVE_WITH_KNOTS('',3,(#8567,#8568,#8569,#8570,#8571,#8572,
#8573,#8574,#8575,#8576,#8577,#8578,#8579,#8580,#8581,#8582,#8583,#8584,
#8585,#8586,#8587,#8588,#8589,#8590,#8591,#8592,#8593,#8594,#8595,#8596,
#8597,#8598,#8599,#8600,#8601,#8602,#8603,#8604,#8605,#8606,#8607,#8608,
#8609,#8610,#8611,#8612,#8613,#8614,#8615,#8616,#8617,#8618,#8619,#8620,
#8621,#8622,#8623,#8624,#8625,#8626,#8627,#8628,#8629,#8630,#8631),
 .UNSPECIFIED.,.F.,.F.,(4,1,1,1,1,1,1,1,1,1,1,1,1,1,1,1,1,1,1,1,1,1,1,1,
1,1,1,1,1,1,1,1,1,1,1,1,1,1,1,1,1,1,1,1,1,1,1,1,1,1,1,1,1,1,1,1,1,1,1,1,
1,1,4),(0.,0.0178571428571429,0.0357142857142857,0.0535714285714286,0.0714285714285714,
0.0892857142857143,0.107142857142857,0.125,0.142857142857143,0.158730158730159,
0.174603174603175,0.19047619047619,0.202380952380952,0.214285714285714,
0.226190476190476,0.238095238095238,0.25,0.261904761904762,0.273809523809524,
0.285714285714286,0.30952380952381,0.333333333333333,0.357142857142857,
0.380952380952381,0.404761904761905,0.428571428571429,0.446428571428571,
0.464285714285714,0.482142857142857,0.5,0.508928571428571,0.517857142857143,
0.535714285714286,0.553571428571429,0.571428571428571,0.589285714285714,
0.607142857142857,0.625,0.642857142857143,0.660714285714286,0.678571428571428,
0.696428571428571,0.714285714285714,0.738095238095238,0.75,0.761904761904762,
0.773809523809524,0.785714285714286,0.797619047619047,0.809523809523809,
0.821428571428571,0.833333333333333,0.845238095238095,0.857142857142857,
0.866071428571429,0.875,0.892857142857143,0.910714285714286,0.928571428571429,
0.946428571428571,0.964285714285714,0.982142857142857,1.),.UNSPECIFIED.);
#222=B_SPLINE_CURVE_WITH_KNOTS('',3,(#8878,#8879,#8880,#8881,#8882,#8883,
#8884,#8885,#8886,#8887,#8888,#8889,#8890,#8891,#8892,#8893,#8894,#8895,
#8896,#8897,#8898,#8899),.UNSPECIFIED.,.F.,.F.,(4,2,2,2,2,2,2,2,2,2,4),
(0.0473477652366656,0.126350602536658,0.189525903804987,0.252701205073317,
0.313298422430275,0.373895639787233,0.434492857144191,0.495090074501149,
0.558265375769478,0.621440677037807,0.7004435143378),.UNSPECIFIED.);
#223=B_SPLINE_CURVE_WITH_KNOTS('',3,(#8903,#8904,#8905,#8906,#8907,#8908,
#8909,#8910,#8911,#8912,#8913,#8914,#8915,#8916,#8917,#8918,#8919,#8920,
#8921,#8922,#8923,#8924),.UNSPECIFIED.,.F.,.F.,(4,2,2,2,2,2,2,2,2,2,4),
(0.0464897534940957,0.0852567806515119,0.170513561303024,0.246687263103517,
0.308657850341199,0.370628437578881,0.432599024816563,0.494569612054245,
0.570743313854739,0.656000094506251,0.694767121663666),.UNSPECIFIED.);
#224=B_SPLINE_CURVE_WITH_KNOTS('',3,(#8930,#8931,#8932,#8933,#8934,#8935,
#8936,#8937,#8938,#8939,#8940,#8941,#8942,#8943,#8944,#8945,#8946,#8947,
#8948,#8949,#8950,#8951),.UNSPECIFIED.,.F.,.F.,(4,2,2,2,2,2,2,2,2,2,4),
(0.0464897534940957,0.0852567806515118,0.170513561303024,0.246687263103517,
0.308657850341199,0.370628437578881,0.432599024816563,0.494569612054245,
0.570743313854738,0.65600009450625,0.694767121663666),.UNSPECIFIED.);
#225=B_SPLINE_CURVE_WITH_KNOTS('',3,(#8955,#8956,#8957,#8958,#8959,#8960,
#8961,#8962,#8963,#8964,#8965,#8966,#8967,#8968,#8969,#8970,#8971,#8972,
#8973,#8974,#8975,#8976),.UNSPECIFIED.,.F.,.F.,(4,2,2,2,2,2,2,2,2,2,4),
(0.0464897534940957,0.0852567806515119,0.170513561303024,0.246687263103517,
0.308657850341199,0.370628437578881,0.432599024816563,0.494569612054245,
0.570743313854739,0.656000094506251,0.694767121663666),.UNSPECIFIED.);
#226=B_SPLINE_CURVE_WITH_KNOTS('',3,(#8980,#8981,#8982,#8983,#8984,#8985,
#8986,#8987,#8988,#8989,#8990,#8991),.UNSPECIFIED.,.F.,.F.,(4,2,2,2,2,4),
(0.0464897534940957,0.0852567806515119,0.170513561303024,0.246687263103517,
0.308657850341199,0.370628437578881),.UNSPECIFIED.);
#227=B_SPLINE_CURVE_WITH_KNOTS('',3,(#8996,#8997,#8998,#8999,#9000,#9001,
#9002,#9003,#9004,#9005,#9006,#9007),.UNSPECIFIED.,.F.,.F.,(4,2,2,2,2,4),
(0.370628437578881,0.432599024816563,0.494569612054245,0.570743313854738,
0.65600009450625,0.694767121663666),.UNSPECIFIED.);
#228=B_SPLINE_CURVE_WITH_KNOTS('',3,(#9011,#9012,#9013,#9014,#9015,#9016,
#9017,#9018,#9019,#9020,#9021,#9022,#9023,#9024,#9025,#9026,#9027,#9028,
#9029,#9030,#9031,#9032),.UNSPECIFIED.,.F.,.F.,(4,2,2,2,2,2,2,2,2,2,4),
(0.0464897534940957,0.0852567806515121,0.170513561303024,0.246687263103518,
0.308657850341199,0.370628437578881,0.432599024816563,0.494569612054245,
0.570743313854738,0.65600009450625,0.694767121663666),.UNSPECIFIED.);
#229=B_SPLINE_CURVE_WITH_KNOTS('',3,(#9036,#9037,#9038,#9039,#9040,#9041,
#9042,#9043,#9044,#9045,#9046,#9047,#9048,#9049,#9050,#9051,#9052,#9053,
#9054,#9055,#9056,#9057),.UNSPECIFIED.,.F.,.F.,(4,2,2,2,2,2,2,2,2,2,4),
(0.0464897534940957,0.0852567806515119,0.170513561303024,0.246687263103517,
0.308657850341199,0.370628437578881,0.432599024816563,0.494569612054245,
0.570743313854738,0.65600009450625,0.694767121663667),.UNSPECIFIED.);
#230=B_SPLINE_CURVE_WITH_KNOTS('',3,(#9061,#9062,#9063,#9064,#9065,#9066,
#9067,#9068,#9069,#9070,#9071,#9072,#9073,#9074,#9075,#9076,#9077,#9078,
#9079,#9080,#9081,#9082),.UNSPECIFIED.,.F.,.F.,(4,2,2,2,2,2,2,2,2,2,4),
(0.0464897534940957,0.0852567806515119,0.170513561303024,0.246687263103517,
0.308657850341199,0.370628437578881,0.432599024816563,0.494569612054245,
0.570743313854738,0.65600009450625,0.694767121663666),.UNSPECIFIED.);
#231=B_SPLINE_CURVE_WITH_KNOTS('',3,(#9086,#9087,#9088,#9089,#9090,#9091,
#9092,#9093,#9094,#9095,#9096,#9097,#9098,#9099,#9100,#9101,#9102,#9103,
#9104,#9105,#9106,#9107),.UNSPECIFIED.,.F.,.F.,(4,2,2,2,2,2,2,2,2,2,4),
(0.0464897534940957,0.0852567806515119,0.170513561303024,0.246687263103517,
0.308657850341199,0.370628437578881,0.432599024816563,0.494569612054245,
0.570743313854739,0.656000094506251,0.694767121663667),.UNSPECIFIED.);
#232=B_SPLINE_CURVE_WITH_KNOTS('',3,(#9115,#9116,#9117,#9118,#9119,#9120,
#9121,#9122,#9123,#9124,#9125,#9126,#9127,#9128,#9129,#9130,#9131,#9132,
#9133,#9134,#9135,#9136),.UNSPECIFIED.,.F.,.F.,(4,2,2,2,2,2,2,2,2,2,4),
(0.0473477652366656,0.126350602536658,0.189525903804987,0.252701205073316,
0.313298422430274,0.373895639787232,0.434492857144191,0.495090074501149,
0.558265375769478,0.621440677037807,0.7004435143378),.UNSPECIFIED.);
#233=B_SPLINE_CURVE_WITH_KNOTS('',3,(#9144,#9145,#9146,#9147,#9148,#9149,
#9150,#9151,#9152,#9153,#9154,#9155,#9156,#9157,#9158,#9159,#9160,#9161,
#9162,#9163,#9164,#9165),.UNSPECIFIED.,.F.,.F.,(4,2,2,2,2,2,2,2,2,2,4),
(0.0473477652366656,0.126350602536658,0.189525903804987,0.252701205073317,
0.313298422430275,0.373895639787233,0.434492857144191,0.495090074501149,
0.558265375769478,0.621440677037807,0.7004435143378),.UNSPECIFIED.);
#234=B_SPLINE_CURVE_WITH_KNOTS('',3,(#9174,#9175,#9176,#9177,#9178,#9179,
#9180,#9181,#9182,#9183,#9184,#9185),.UNSPECIFIED.,.F.,.F.,(4,2,2,2,2,4),
(0.0473477652366656,0.126350602536658,0.189525903804987,0.252701205073316,
0.313298422430275,0.373895639787233),.UNSPECIFIED.);
#235=B_SPLINE_CURVE_WITH_KNOTS('',3,(#9187,#9188,#9189,#9190,#9191,#9192,
#9193,#9194,#9195,#9196,#9197,#9198),.UNSPECIFIED.,.F.,.F.,(4,2,2,2,2,4),
(0.373895639787233,0.434492857144191,0.495090074501149,0.558265375769478,
0.621440677037807,0.7004435143378),.UNSPECIFIED.);
#236=B_SPLINE_CURVE_WITH_KNOTS('',3,(#9205,#9206,#9207,#9208,#9209,#9210,
#9211,#9212,#9213,#9214,#9215,#9216,#9217,#9218,#9219,#9220,#9221,#9222,
#9223,#9224,#9225,#9226),.UNSPECIFIED.,.F.,.F.,(4,2,2,2,2,2,2,2,2,2,4),
(0.0473477652366656,0.126350602536658,0.189525903804987,0.252701205073316,
0.313298422430275,0.373895639787233,0.434492857144191,0.495090074501149,
0.558265375769478,0.621440677037807,0.7004435143378),.UNSPECIFIED.);
#237=B_SPLINE_CURVE_WITH_KNOTS('',3,(#9234,#9235,#9236,#9237,#9238,#9239,
#9240,#9241,#9242,#9243,#9244,#9245,#9246,#9247,#9248,#9249,#9250,#9251,
#9252,#9253,#9254,#9255),.UNSPECIFIED.,.F.,.F.,(4,2,2,2,2,2,2,2,2,2,4),
(0.0473477652366656,0.126350602536658,0.189525903804987,0.252701205073317,
0.313298422430275,0.373895639787233,0.434492857144191,0.495090074501149,
0.558265375769478,0.621440677037807,0.7004435143378),.UNSPECIFIED.);
#238=B_SPLINE_CURVE_WITH_KNOTS('',3,(#9263,#9264,#9265,#9266,#9267,#9268,
#9269,#9270,#9271,#9272,#9273,#9274,#9275,#9276,#9277,#9278,#9279,#9280,
#9281,#9282,#9283,#9284),.UNSPECIFIED.,.F.,.F.,(4,2,2,2,2,2,2,2,2,2,4),
(0.0473477652366656,0.126350602536658,0.189525903804987,0.252701205073316,
0.313298422430275,0.373895639787233,0.434492857144191,0.495090074501149,
0.558265375769478,0.621440677037807,0.7004435143378),.UNSPECIFIED.);
#239=B_SPLINE_CURVE_WITH_KNOTS('',3,(#9293,#9294,#9295,#9296,#9297,#9298,
#9299,#9300,#9301,#9302,#9303,#9304,#9305,#9306,#9307,#9308,#9309,#9310,
#9311,#9312,#9313,#9314),.UNSPECIFIED.,.F.,.F.,(4,2,2,2,2,2,2,2,2,2,4),
(0.0473477652366656,0.126350602536658,0.189525903804987,0.252701205073317,
0.313298422430275,0.373895639787233,0.434492857144191,0.495090074501149,
0.558265375769478,0.621440677037807,0.7004435143378),.UNSPECIFIED.);
#240=B_SPLINE_CURVE_WITH_KNOTS('',3,(#9473,#9474,#9475,#9476,#9477,#9478,
#9479,#9480,#9481,#9482,#9483,#9484,#9485,#9486,#9487,#9488,#9489,#9490,
#9491,#9492,#9493,#9494,#9495,#9496,#9497,#9498,#9499,#9500,#9501,#9502,
#9503,#9504,#9505,#9506,#9507,#9508,#9509,#9510,#9511,#9512,#9513,#9514),
 .UNSPECIFIED.,.T.,.F.,(4,2,2,2,2,2,2,2,2,2,2,2,2,2,2,2,2,2,2,2,4),(0.,
0.0839475318916269,0.12592129783744,0.167895063783254,0.205982250035365,
0.244069436287477,0.282156622539588,0.320243808791699,0.362217574737513,
0.404191340683327,0.488138872574954,0.572086404466582,0.614060170412395,
0.656033936358209,0.694121122610321,0.732208308862432,0.770295495114543,
0.808382681366655,0.850356447312468,0.892330213258282,0.976277745149909),
 .UNSPECIFIED.);
#241=B_SPLINE_SURFACE_WITH_KNOTS('',3,3,((#7914,#7915,#7916,#7917,#7918,
#7919,#7920,#7921,#7922,#7923,#7924,#7925,#7926,#7927,#7928,#7929,#7930,
#7931,#7932,#7933,#7934,#7935,#7936,#7937,#7938,#7939,#7940,#7941,#7942,
#7943,#7944,#7945,#7946,#7947,#7948,#7949,#7950,#7951,#7952,#7953,#7954,
#7955,#7956,#7957,#7958,#7959,#7960,#7961,#7962,#7963,#7964,#7965,#7966,
#7967,#7968,#7969,#7970,#7971,#7972,#7973,#7974,#7975,#7976,#7977,#7978),
(#7979,#7980,#7981,#7982,#7983,#7984,#7985,#7986,#7987,#7988,#7989,#7990,
#7991,#7992,#7993,#7994,#7995,#7996,#7997,#7998,#7999,#8000,#8001,#8002,
#8003,#8004,#8005,#8006,#8007,#8008,#8009,#8010,#8011,#8012,#8013,#8014,
#8015,#8016,#8017,#8018,#8019,#8020,#8021,#8022,#8023,#8024,#8025,#8026,
#8027,#8028,#8029,#8030,#8031,#8032,#8033,#8034,#8035,#8036,#8037,#8038,
#8039,#8040,#8041,#8042,#8043),(#8044,#8045,#8046,#8047,#8048,#8049,#8050,
#8051,#8052,#8053,#8054,#8055,#8056,#8057,#8058,#8059,#8060,#8061,#8062,
#8063,#8064,#8065,#8066,#8067,#8068,#8069,#8070,#8071,#8072,#8073,#8074,
#8075,#8076,#8077,#8078,#8079,#8080,#8081,#8082,#8083,#8084,#8085,#8086,
#8087,#8088,#8089,#8090,#8091,#8092,#8093,#8094,#8095,#8096,#8097,#8098,
#8099,#8100,#8101,#8102,#8103,#8104,#8105,#8106,#8107,#8108),(#8109,#8110,
#8111,#8112,#8113,#8114,#8115,#8116,#8117,#8118,#8119,#8120,#8121,#8122,
#8123,#8124,#8125,#8126,#8127,#8128,#8129,#8130,#8131,#8132,#8133,#8134,
#8135,#8136,#8137,#8138,#8139,#8140,#8141,#8142,#8143,#8144,#8145,#8146,
#8147,#8148,#8149,#8150,#8151,#8152,#8153,#8154,#8155,#8156,#8157,#8158,
#8159,#8160,#8161,#8162,#8163,#8164,#8165,#8166,#8167,#8168,#8169,#8170,
#8171,#8172,#8173),(#8174,#8175,#8176,#8177,#8178,#8179,#8180,#8181,#8182,
#8183,#8184,#8185,#8186,#8187,#8188,#8189,#8190,#8191,#8192,#8193,#8194,
#8195,#8196,#8197,#8198,#8199,#8200,#8201,#8202,#8203,#8204,#8205,#8206,
#8207,#8208,#8209,#8210,#8211,#8212,#8213,#8214,#8215,#8216,#8217,#8218,
#8219,#8220,#8221,#8222,#8223,#8224,#8225,#8226,#8227,#8228,#8229,#8230,
#8231,#8232,#8233,#8234,#8235,#8236,#8237,#8238),(#8239,#8240,#8241,#8242,
#8243,#8244,#8245,#8246,#8247,#8248,#8249,#8250,#8251,#8252,#8253,#8254,
#8255,#8256,#8257,#8258,#8259,#8260,#8261,#8262,#8263,#8264,#8265,#8266,
#8267,#8268,#8269,#8270,#8271,#8272,#8273,#8274,#8275,#8276,#8277,#8278,
#8279,#8280,#8281,#8282,#8283,#8284,#8285,#8286,#8287,#8288,#8289,#8290,
#8291,#8292,#8293,#8294,#8295,#8296,#8297,#8298,#8299,#8300,#8301,#8302,
#8303),(#8304,#8305,#8306,#8307,#8308,#8309,#8310,#8311,#8312,#8313,#8314,
#8315,#8316,#8317,#8318,#8319,#8320,#8321,#8322,#8323,#8324,#8325,#8326,
#8327,#8328,#8329,#8330,#8331,#8332,#8333,#8334,#8335,#8336,#8337,#8338,
#8339,#8340,#8341,#8342,#8343,#8344,#8345,#8346,#8347,#8348,#8349,#8350,
#8351,#8352,#8353,#8354,#8355,#8356,#8357,#8358,#8359,#8360,#8361,#8362,
#8363,#8364,#8365,#8366,#8367,#8368),(#8369,#8370,#8371,#8372,#8373,#8374,
#8375,#8376,#8377,#8378,#8379,#8380,#8381,#8382,#8383,#8384,#8385,#8386,
#8387,#8388,#8389,#8390,#8391,#8392,#8393,#8394,#8395,#8396,#8397,#8398,
#8399,#8400,#8401,#8402,#8403,#8404,#8405,#8406,#8407,#8408,#8409,#8410,
#8411,#8412,#8413,#8414,#8415,#8416,#8417,#8418,#8419,#8420,#8421,#8422,
#8423,#8424,#8425,#8426,#8427,#8428,#8429,#8430,#8431,#8432,#8433),(#8434,
#8435,#8436,#8437,#8438,#8439,#8440,#8441,#8442,#8443,#8444,#8445,#8446,
#8447,#8448,#8449,#8450,#8451,#8452,#8453,#8454,#8455,#8456,#8457,#8458,
#8459,#8460,#8461,#8462,#8463,#8464,#8465,#8466,#8467,#8468,#8469,#8470,
#8471,#8472,#8473,#8474,#8475,#8476,#8477,#8478,#8479,#8480,#8481,#8482,
#8483,#8484,#8485,#8486,#8487,#8488,#8489,#8490,#8491,#8492,#8493,#8494,
#8495,#8496,#8497,#8498),(#8499,#8500,#8501,#8502,#8503,#8504,#8505,#8506,
#8507,#8508,#8509,#8510,#8511,#8512,#8513,#8514,#8515,#8516,#8517,#8518,
#8519,#8520,#8521,#8522,#8523,#8524,#8525,#8526,#8527,#8528,#8529,#8530,
#8531,#8532,#8533,#8534,#8535,#8536,#8537,#8538,#8539,#8540,#8541,#8542,
#8543,#8544,#8545,#8546,#8547,#8548,#8549,#8550,#8551,#8552,#8553,#8554,
#8555,#8556,#8557,#8558,#8559,#8560,#8561,#8562,#8563)),.UNSPECIFIED.,.T.,
 .F.,.F.,(4,1,1,1,1,1,1,4),(4,1,1,1,1,1,1,1,1,1,1,1,1,1,1,1,1,1,1,1,1,1,
1,1,1,1,1,1,1,1,1,1,1,1,1,1,1,1,1,1,1,1,1,1,1,1,1,1,1,1,1,1,1,1,1,1,1,1,
1,1,1,1,4),(-3.14159265358979,-2.24399475256414,-1.34639685153848,-0.448798950512828,
0.448798950512828,1.34639685153848,2.24399475256414,3.14159265358979),(0.,
0.0178571428571429,0.0357142857142857,0.0535714285714286,0.0714285714285714,
0.0892857142857143,0.107142857142857,0.125,0.142857142857143,0.158730158730159,
0.174603174603175,0.19047619047619,0.202380952380952,0.214285714285714,
0.226190476190476,0.238095238095238,0.25,0.261904761904762,0.273809523809524,
0.285714285714286,0.30952380952381,0.333333333333333,0.357142857142857,
0.380952380952381,0.404761904761905,0.428571428571429,0.446428571428571,
0.464285714285714,0.482142857142857,0.5,0.508928571428571,0.517857142857143,
0.535714285714286,0.553571428571429,0.571428571428571,0.589285714285714,
0.607142857142857,0.625,0.642857142857143,0.660714285714286,0.678571428571428,
0.696428571428571,0.714285714285714,0.738095238095238,0.75,0.761904761904762,
0.773809523809524,0.785714285714286,0.797619047619047,0.809523809523809,
0.821428571428571,0.833333333333333,0.845238095238095,0.857142857142857,
0.866071428571429,0.875,0.892857142857143,0.910714285714286,0.928571428571429,
0.946428571428571,0.964285714285714,0.982142857142857,1.),.UNSPECIFIED.);
#242=SPHERICAL_SURFACE('',#5356,0.3);
#243=SPHERICAL_SURFACE('',#5484,0.23815);
#244=SPHERICAL_SURFACE('',#5486,0.23815);
#245=SPHERICAL_SURFACE('',#5488,0.23815);
#246=SPHERICAL_SURFACE('',#5490,0.23815);
#247=SPHERICAL_SURFACE('',#5492,0.23815);
#248=SPHERICAL_SURFACE('',#5494,0.23815);
#249=SPHERICAL_SURFACE('',#5496,0.23815);
#250=SPHERICAL_SURFACE('',#5498,0.23815);
#251=SPHERICAL_SURFACE('',#5501,0.247676);
#252=SPHERICAL_SURFACE('',#5517,0.247676);
#253=SPHERICAL_SURFACE('',#5522,0.247676);
#254=SPHERICAL_SURFACE('',#5527,0.247676);
#255=SPHERICAL_SURFACE('',#5532,0.247676);
#256=SPHERICAL_SURFACE('',#5537,0.247676);
#257=SPHERICAL_SURFACE('',#5542,0.247676);
#258=SPHERICAL_SURFACE('',#5550,0.247676);
#259=SPHERICAL_SURFACE('',#5643,0.3);
#260=SHAPE_REPRESENTATION_RELATIONSHIP('SRR','None',#9937,#291);
#261=SHAPE_REPRESENTATION_RELATIONSHIP('SRR','None',#9938,#292);
#262=SHAPE_REPRESENTATION_RELATIONSHIP('SRR','None',#9939,#293);
#263=SHAPE_REPRESENTATION_RELATIONSHIP('SRR','None',#9940,#294);
#264=SHAPE_REPRESENTATION_RELATIONSHIP('SRR','None',#9941,#295);
#265=SHAPE_REPRESENTATION_RELATIONSHIP('SRR','None',#9942,#296);
#266=SHAPE_REPRESENTATION_RELATIONSHIP('SRR','None',#9943,#297);
#267=SHAPE_REPRESENTATION_RELATIONSHIP('SRR','None',#9944,#298);
#268=SHAPE_REPRESENTATION_RELATIONSHIP('SRR','None',#9945,#299);
#269=SHAPE_REPRESENTATION_RELATIONSHIP('SRR','None',#9946,#300);
#270=SHAPE_REPRESENTATION_RELATIONSHIP('SRR','None',#9947,#301);
#271=SHAPE_REPRESENTATION_RELATIONSHIP('SRR','None',#9948,#302);
#272=SHAPE_REPRESENTATION_RELATIONSHIP('SRR','None',#9949,#303);
#273=SHAPE_REPRESENTATION_RELATIONSHIP('SRR','None',#9950,#304);
#274=SHAPE_REPRESENTATION_RELATIONSHIP('SRR','None',#9951,#305);
#275=SHAPE_REPRESENTATION_RELATIONSHIP('SRR','None',#9952,#306);
#276=SHAPE_REPRESENTATION_RELATIONSHIP('SRR','None',#9953,#307);
#277=SHAPE_REPRESENTATION_RELATIONSHIP('SRR','None',#9954,#308);
#278=SHAPE_REPRESENTATION_RELATIONSHIP('SRR','None',#9955,#309);
#279=SHAPE_REPRESENTATION_RELATIONSHIP('SRR','None',#9957,#310);
#280=SHAPE_REPRESENTATION_RELATIONSHIP('SRR','None',#9958,#311);
#281=SHAPE_REPRESENTATION_RELATIONSHIP('SRR','None',#9959,#312);
#282=SHAPE_REPRESENTATION_RELATIONSHIP('SRR','None',#9960,#313);
#283=SHAPE_REPRESENTATION_RELATIONSHIP('SRR','None',#9961,#314);
#284=SHAPE_REPRESENTATION_RELATIONSHIP('SRR','None',#9962,#315);
#285=SHAPE_REPRESENTATION_RELATIONSHIP('SRR','None',#9964,#316);
#286=SHAPE_REPRESENTATION_RELATIONSHIP('SRR','None',#9965,#317);
#287=SHAPE_REPRESENTATION_RELATIONSHIP('SRR','None',#9966,#318);
#288=SHAPE_REPRESENTATION_RELATIONSHIP('SRR','None',#9967,#319);
#289=SHAPE_REPRESENTATION_RELATIONSHIP('SRR','None',#9968,#320);
#290=SHAPE_REPRESENTATION_RELATIONSHIP('SRR','None',#9969,#321);
#291=ADVANCED_BREP_SHAPE_REPRESENTATION('',(#362),#9780);
#292=ADVANCED_BREP_SHAPE_REPRESENTATION('',(#363),#9781);
#293=ADVANCED_BREP_SHAPE_REPRESENTATION('',(#364),#9782);
#294=ADVANCED_BREP_SHAPE_REPRESENTATION('',(#365,#366),#9783);
#295=ADVANCED_BREP_SHAPE_REPRESENTATION('',(#367),#9784);
#296=ADVANCED_BREP_SHAPE_REPRESENTATION('',(#368),#9785);
#297=ADVANCED_BREP_SHAPE_REPRESENTATION('',(#369),#9786);
#298=ADVANCED_BREP_SHAPE_REPRESENTATION('',(#370),#9787);
#299=ADVANCED_BREP_SHAPE_REPRESENTATION('',(#371),#9788);
#300=ADVANCED_BREP_SHAPE_REPRESENTATION('',(#372),#9789);
#301=ADVANCED_BREP_SHAPE_REPRESENTATION('',(#373),#9790);
#302=ADVANCED_BREP_SHAPE_REPRESENTATION('',(#374),#9791);
#303=ADVANCED_BREP_SHAPE_REPRESENTATION('',(#375),#9792);
#304=ADVANCED_BREP_SHAPE_REPRESENTATION('',(#376),#9793);
#305=ADVANCED_BREP_SHAPE_REPRESENTATION('',(#377),#9794);
#306=ADVANCED_BREP_SHAPE_REPRESENTATION('',(#378),#9795);
#307=ADVANCED_BREP_SHAPE_REPRESENTATION('',(#379),#9796);
#308=ADVANCED_BREP_SHAPE_REPRESENTATION('',(#380),#9797);
#309=ADVANCED_BREP_SHAPE_REPRESENTATION('',(#218),#9798);
#310=ADVANCED_BREP_SHAPE_REPRESENTATION('',(#381),#9800);
#311=ADVANCED_BREP_SHAPE_REPRESENTATION('',(#382),#9801);
#312=ADVANCED_BREP_SHAPE_REPRESENTATION('',(#383,#384,#385,#386,#387,#388,
#389,#390),#9802);
#313=ADVANCED_BREP_SHAPE_REPRESENTATION('',(#391),#9803);
#314=ADVANCED_BREP_SHAPE_REPRESENTATION('',(#392,#393),#9804);
#315=ADVANCED_BREP_SHAPE_REPRESENTATION('',(#219),#9805);
#316=ADVANCED_BREP_SHAPE_REPRESENTATION('',(#394),#9807);
#317=ADVANCED_BREP_SHAPE_REPRESENTATION('',(#395),#9808);
#318=ADVANCED_BREP_SHAPE_REPRESENTATION('',(#396),#9809);
#319=ADVANCED_BREP_SHAPE_REPRESENTATION('',(#397),#9810);
#320=ADVANCED_BREP_SHAPE_REPRESENTATION('',(#398),#9811);
#321=ADVANCED_BREP_SHAPE_REPRESENTATION('',(#220),#9812);
#322=STYLED_ITEM('',(#10162),#362);
#323=STYLED_ITEM('',(#10169),#363);
#324=STYLED_ITEM('',(#10169),#364);
#325=STYLED_ITEM('',(#10169),#365);
#326=STYLED_ITEM('',(#10169),#366);
#327=STYLED_ITEM('',(#10176),#367);
#328=STYLED_ITEM('',(#10183),#368);
#329=STYLED_ITEM('',(#10183),#369);
#330=STYLED_ITEM('',(#10183),#370);
#331=STYLED_ITEM('',(#10183),#371);
#332=STYLED_ITEM('',(#10176),#372);
#333=STYLED_ITEM('',(#10197),#373);
#334=STYLED_ITEM('',(#10183),#374);
#335=STYLED_ITEM('',(#10183),#375);
#336=STYLED_ITEM('',(#10169),#376);
#337=STYLED_ITEM('',(#10183),#377);
#338=STYLED_ITEM('',(#10169),#378);
#339=STYLED_ITEM('',(#10197),#379);
#340=STYLED_ITEM('',(#10190),#380);
#341=STYLED_ITEM('',(#10190),#218);
#342=STYLED_ITEM('',(#10183),#381);
#343=STYLED_ITEM('',(#10183),#382);
#344=STYLED_ITEM('',(#10183),#383);
#345=STYLED_ITEM('',(#10183),#384);
#346=STYLED_ITEM('',(#10183),#385);
#347=STYLED_ITEM('',(#10183),#386);
#348=STYLED_ITEM('',(#10183),#387);
#349=STYLED_ITEM('',(#10183),#388);
#350=STYLED_ITEM('',(#10183),#389);
#351=STYLED_ITEM('',(#10183),#390);
#352=STYLED_ITEM('',(#10183),#391);
#353=STYLED_ITEM('',(#10183),#392);
#354=STYLED_ITEM('',(#10183),#393);
#355=STYLED_ITEM('',(#10190),#219);
#356=STYLED_ITEM('',(#10183),#394);
#357=STYLED_ITEM('',(#10183),#395);
#358=STYLED_ITEM('',(#10183),#396);
#359=STYLED_ITEM('',(#10183),#397);
#360=STYLED_ITEM('',(#10183),#398);
#361=STYLED_ITEM('',(#10190),#220);
#362=MANIFOLD_SOLID_BREP('Body1',#4753);
#363=MANIFOLD_SOLID_BREP('Body1',#4754);
#364=MANIFOLD_SOLID_BREP('Body1',#4755);
#365=MANIFOLD_SOLID_BREP('Body1',#4756);
#366=MANIFOLD_SOLID_BREP('Body2',#4757);
#367=MANIFOLD_SOLID_BREP('Body1',#4758);
#368=MANIFOLD_SOLID_BREP('Body1',#4759);
#369=MANIFOLD_SOLID_BREP('Body1',#4760);
#370=MANIFOLD_SOLID_BREP('Body1',#4761);
#371=MANIFOLD_SOLID_BREP('Body1',#4762);
#372=MANIFOLD_SOLID_BREP('Body1',#4763);
#373=MANIFOLD_SOLID_BREP('Body1',#4764);
#374=MANIFOLD_SOLID_BREP('Body1',#4765);
#375=MANIFOLD_SOLID_BREP('Body1',#4766);
#376=MANIFOLD_SOLID_BREP('Body1',#4767);
#377=MANIFOLD_SOLID_BREP('Body1',#4768);
#378=MANIFOLD_SOLID_BREP('Body1',#4769);
#379=MANIFOLD_SOLID_BREP('Body1',#4770);
#380=MANIFOLD_SOLID_BREP('Body1',#4771);
#381=MANIFOLD_SOLID_BREP('Body1',#4774);
#382=MANIFOLD_SOLID_BREP('Body1',#4775);
#383=MANIFOLD_SOLID_BREP('Body1',#4776);
#384=MANIFOLD_SOLID_BREP('Body2',#4777);
#385=MANIFOLD_SOLID_BREP('Body3',#4778);
#386=MANIFOLD_SOLID_BREP('Body4',#4779);
#387=MANIFOLD_SOLID_BREP('Body5',#4780);
#388=MANIFOLD_SOLID_BREP('Body6',#4781);
#389=MANIFOLD_SOLID_BREP('Body7',#4782);
#390=MANIFOLD_SOLID_BREP('Body8',#4783);
#391=MANIFOLD_SOLID_BREP('Continuous crown cage',#4784);
#392=MANIFOLD_SOLID_BREP('Body1',#4785);
#393=MANIFOLD_SOLID_BREP('Body2',#4786);
#394=MANIFOLD_SOLID_BREP('Body1',#4789);
#395=MANIFOLD_SOLID_BREP('Body1',#4790);
#396=MANIFOLD_SOLID_BREP('Body1',#4791);
#397=MANIFOLD_SOLID_BREP('Body1',#4792);
#398=MANIFOLD_SOLID_BREP('Body1',#4793);
#399=FACE_BOUND('',#957,.T.);
#400=FACE_BOUND('',#958,.T.);
#401=FACE_BOUND('',#959,.T.);
#402=FACE_BOUND('',#960,.T.);
#403=FACE_BOUND('',#962,.T.);
#404=FACE_BOUND('',#963,.T.);
#405=FACE_BOUND('',#964,.T.);
#406=FACE_BOUND('',#965,.T.);
#407=FACE_BOUND('',#993,.T.);
#408=FACE_BOUND('',#994,.T.);
#409=FACE_BOUND('',#995,.T.);
#410=FACE_BOUND('',#996,.T.);
#411=FACE_BOUND('',#998,.T.);
#412=FACE_BOUND('',#999,.T.);
#413=FACE_BOUND('',#1000,.T.);
#414=FACE_BOUND('',#1001,.T.);
#415=FACE_BOUND('',#1007,.T.);
#416=FACE_BOUND('',#1008,.T.);
#417=FACE_BOUND('',#1009,.T.);
#418=FACE_BOUND('',#1010,.T.);
#419=FACE_BOUND('',#1013,.T.);
#420=FACE_BOUND('',#1014,.T.);
#421=FACE_BOUND('',#1015,.T.);
#422=FACE_BOUND('',#1016,.T.);
#423=FACE_BOUND('',#1025,.T.);
#424=FACE_BOUND('',#1028,.T.);
#425=FACE_BOUND('',#1029,.T.);
#426=FACE_BOUND('',#1030,.T.);
#427=FACE_BOUND('',#1031,.T.);
#428=FACE_BOUND('',#1037,.T.);
#429=FACE_BOUND('',#1038,.T.);
#430=FACE_BOUND('',#1039,.T.);
#431=FACE_BOUND('',#1040,.T.);
#432=FACE_BOUND('',#1042,.T.);
#433=FACE_BOUND('',#1045,.T.);
#434=FACE_BOUND('',#1048,.T.);
#435=FACE_BOUND('',#1056,.T.);
#436=FACE_BOUND('',#1058,.T.);
#437=FACE_BOUND('',#1059,.T.);
#438=FACE_BOUND('',#1060,.T.);
#439=FACE_BOUND('',#1061,.T.);
#440=FACE_BOUND('',#1067,.T.);
#441=FACE_BOUND('',#1070,.T.);
#442=FACE_BOUND('',#1071,.T.);
#443=FACE_BOUND('',#1072,.T.);
#444=FACE_BOUND('',#1073,.T.);
#445=FACE_BOUND('',#1079,.T.);
#446=FACE_BOUND('',#1080,.T.);
#447=FACE_BOUND('',#1081,.T.);
#448=FACE_BOUND('',#1082,.T.);
#449=FACE_BOUND('',#1085,.T.);
#450=FACE_BOUND('',#1088,.T.);
#451=FACE_BOUND('',#1091,.T.);
#452=FACE_BOUND('',#1093,.T.);
#453=FACE_BOUND('',#1100,.T.);
#454=FACE_BOUND('',#1101,.T.);
#455=FACE_BOUND('',#1102,.T.);
#456=FACE_BOUND('',#1103,.T.);
#457=FACE_BOUND('',#1114,.T.);
#458=FACE_BOUND('',#1117,.T.);
#459=FACE_BOUND('',#1121,.T.);
#460=FACE_BOUND('',#1127,.T.);
#461=FACE_BOUND('',#1130,.T.);
#462=FACE_BOUND('',#1134,.T.);
#463=FACE_BOUND('',#1138,.T.);
#464=FACE_BOUND('',#1140,.T.);
#465=FACE_BOUND('',#1159,.T.);
#466=FACE_BOUND('',#1161,.T.);
#467=FACE_BOUND('',#1176,.T.);
#468=FACE_BOUND('',#1184,.T.);
#469=FACE_BOUND('',#1187,.T.);
#470=FACE_BOUND('',#1192,.T.);
#471=FACE_BOUND('',#1197,.T.);
#472=FACE_BOUND('',#1225,.T.);
#473=FACE_BOUND('',#1228,.T.);
#474=FACE_BOUND('',#1231,.T.);
#475=FACE_BOUND('',#1234,.T.);
#476=FACE_BOUND('',#1237,.T.);
#477=FACE_BOUND('',#1253,.T.);
#478=FACE_BOUND('',#1263,.T.);
#479=FACE_BOUND('',#1266,.T.);
#480=FACE_BOUND('',#1267,.T.);
#481=FACE_BOUND('',#1268,.T.);
#482=FACE_BOUND('',#1269,.T.);
#483=FACE_BOUND('',#1276,.T.);
#484=FACE_BOUND('',#1277,.T.);
#485=FACE_BOUND('',#1278,.T.);
#486=FACE_BOUND('',#1279,.T.);
#487=FACE_BOUND('',#1283,.T.);
#488=FACE_BOUND('',#1285,.T.);
#489=FACE_BOUND('',#1289,.T.);
#490=FACE_BOUND('',#1291,.T.);
#491=FACE_BOUND('',#1295,.T.);
#492=FACE_BOUND('',#1297,.T.);
#493=FACE_BOUND('',#1301,.T.);
#494=FACE_BOUND('',#1303,.T.);
#495=FACE_BOUND('',#1307,.T.);
#496=FACE_BOUND('',#1309,.T.);
#497=FACE_BOUND('',#1313,.T.);
#498=FACE_BOUND('',#1315,.T.);
#499=FACE_BOUND('',#1321,.T.);
#500=PLANE('',#5153);
#501=PLANE('',#5154);
#502=PLANE('',#5155);
#503=PLANE('',#5156);
#504=PLANE('',#5157);
#505=PLANE('',#5158);
#506=PLANE('',#5160);
#507=PLANE('',#5161);
#508=PLANE('',#5162);
#509=PLANE('',#5163);
#510=PLANE('',#5164);
#511=PLANE('',#5165);
#512=PLANE('',#5167);
#513=PLANE('',#5168);
#514=PLANE('',#5169);
#515=PLANE('',#5170);
#516=PLANE('',#5171);
#517=PLANE('',#5172);
#518=PLANE('',#5174);
#519=PLANE('',#5175);
#520=PLANE('',#5176);
#521=PLANE('',#5177);
#522=PLANE('',#5178);
#523=PLANE('',#5179);
#524=PLANE('',#5192);
#525=PLANE('',#5193);
#526=PLANE('',#5194);
#527=PLANE('',#5195);
#528=PLANE('',#5196);
#529=PLANE('',#5197);
#530=PLANE('',#5211);
#531=PLANE('',#5212);
#532=PLANE('',#5213);
#533=PLANE('',#5214);
#534=PLANE('',#5215);
#535=PLANE('',#5216);
#536=PLANE('',#5230);
#537=PLANE('',#5234);
#538=PLANE('',#5236);
#539=PLANE('',#5237);
#540=PLANE('',#5238);
#541=PLANE('',#5241);
#542=PLANE('',#5243);
#543=PLANE('',#5249);
#544=PLANE('',#5255);
#545=PLANE('',#5276);
#546=PLANE('',#5277);
#547=PLANE('',#5291);
#548=PLANE('',#5295);
#549=PLANE('',#5297);
#550=PLANE('',#5298);
#551=PLANE('',#5299);
#552=PLANE('',#5302);
#553=PLANE('',#5307);
#554=PLANE('',#5313);
#555=PLANE('',#5319);
#556=PLANE('',#5322);
#557=PLANE('',#5338);
#558=PLANE('',#5343);
#559=PLANE('',#5344);
#560=PLANE('',#5345);
#561=PLANE('',#5346);
#562=PLANE('',#5347);
#563=PLANE('',#5348);
#564=PLANE('',#5349);
#565=PLANE('',#5350);
#566=PLANE('',#5351);
#567=PLANE('',#5352);
#568=PLANE('',#5353);
#569=PLANE('',#5354);
#570=PLANE('',#5359);
#571=PLANE('',#5366);
#572=PLANE('',#5367);
#573=PLANE('',#5369);
#574=PLANE('',#5374);
#575=PLANE('',#5380);
#576=PLANE('',#5388);
#577=PLANE('',#5389);
#578=PLANE('',#5393);
#579=PLANE('',#5394);
#580=PLANE('',#5396);
#581=PLANE('',#5397);
#582=PLANE('',#5398);
#583=PLANE('',#5399);
#584=PLANE('',#5400);
#585=PLANE('',#5401);
#586=PLANE('',#5403);
#587=PLANE('',#5404);
#588=PLANE('',#5405);
#589=PLANE('',#5406);
#590=PLANE('',#5407);
#591=PLANE('',#5408);
#592=PLANE('',#5416);
#593=PLANE('',#5417);
#594=PLANE('',#5419);
#595=PLANE('',#5420);
#596=PLANE('',#5421);
#597=PLANE('',#5422);
#598=PLANE('',#5423);
#599=PLANE('',#5424);
#600=PLANE('',#5425);
#601=PLANE('',#5426);
#602=PLANE('',#5427);
#603=PLANE('',#5429);
#604=PLANE('',#5437);
#605=PLANE('',#5457);
#606=PLANE('',#5460);
#607=PLANE('',#5472);
#608=PLANE('',#5481);
#609=PLANE('',#5514);
#610=PLANE('',#5519);
#611=PLANE('',#5524);
#612=PLANE('',#5529);
#613=PLANE('',#5534);
#614=PLANE('',#5539);
#615=PLANE('',#5548);
#616=PLANE('',#5552);
#617=PLANE('',#5553);
#618=PLANE('',#5555);
#619=PLANE('',#5560);
#620=PLANE('',#5563);
#621=PLANE('',#5568);
#622=PLANE('',#5577);
#623=PLANE('',#5578);
#624=PLANE('',#5579);
#625=PLANE('',#5580);
#626=PLANE('',#5581);
#627=PLANE('',#5582);
#628=PLANE('',#5583);
#629=PLANE('',#5584);
#630=PLANE('',#5585);
#631=PLANE('',#5587);
#632=PLANE('',#5595);
#633=PLANE('',#5638);
#634=PLANE('',#5642);
#635=PLANE('',#5644);
#636=PLANE('',#5649);
#637=PLANE('',#5651);
#638=PLANE('',#5666);
#639=PLANE('',#5667);
#640=PLANE('',#5670);
#641=PLANE('',#5672);
#642=PLANE('',#5678);
#643=PLANE('',#5679);
#644=PLANE('',#5687);
#645=PLANE('',#5688);
#646=PLANE('',#5696);
#647=PLANE('',#5697);
#648=PLANE('',#5705);
#649=PLANE('',#5706);
#650=PLANE('',#5714);
#651=PLANE('',#5715);
#652=PLANE('',#5717);
#653=PLANE('',#5725);
#654=PLANE('',#5733);
#655=PLANE('',#5734);
#656=PLANE('',#5735);
#657=PLANE('',#5736);
#658=PLANE('',#5737);
#659=PLANE('',#5738);
#660=PLANE('',#5739);
#661=PLANE('',#5740);
#662=PLANE('',#5741);
#663=FACE_OUTER_BOUND('',#948,.T.);
#664=FACE_OUTER_BOUND('',#949,.T.);
#665=FACE_OUTER_BOUND('',#950,.T.);
#666=FACE_OUTER_BOUND('',#951,.T.);
#667=FACE_OUTER_BOUND('',#952,.T.);
#668=FACE_OUTER_BOUND('',#953,.T.);
#669=FACE_OUTER_BOUND('',#954,.T.);
#670=FACE_OUTER_BOUND('',#955,.T.);
#671=FACE_OUTER_BOUND('',#956,.T.);
#672=FACE_OUTER_BOUND('',#961,.T.);
#673=FACE_OUTER_BOUND('',#966,.T.);
#674=FACE_OUTER_BOUND('',#967,.T.);
#675=FACE_OUTER_BOUND('',#968,.T.);
#676=FACE_OUTER_BOUND('',#969,.T.);
#677=FACE_OUTER_BOUND('',#970,.T.);
#678=FACE_OUTER_BOUND('',#971,.T.);
#679=FACE_OUTER_BOUND('',#972,.T.);
#680=FACE_OUTER_BOUND('',#973,.T.);
#681=FACE_OUTER_BOUND('',#974,.T.);
#682=FACE_OUTER_BOUND('',#975,.T.);
#683=FACE_OUTER_BOUND('',#976,.T.);
#684=FACE_OUTER_BOUND('',#977,.T.);
#685=FACE_OUTER_BOUND('',#978,.T.);
#686=FACE_OUTER_BOUND('',#979,.T.);
#687=FACE_OUTER_BOUND('',#980,.T.);
#688=FACE_OUTER_BOUND('',#981,.T.);
#689=FACE_OUTER_BOUND('',#982,.T.);
#690=FACE_OUTER_BOUND('',#983,.T.);
#691=FACE_OUTER_BOUND('',#984,.T.);
#692=FACE_OUTER_BOUND('',#985,.T.);
#693=FACE_OUTER_BOUND('',#986,.T.);
#694=FACE_OUTER_BOUND('',#987,.T.);
#695=FACE_OUTER_BOUND('',#988,.T.);
#696=FACE_OUTER_BOUND('',#989,.T.);
#697=FACE_OUTER_BOUND('',#990,.T.);
#698=FACE_OUTER_BOUND('',#991,.T.);
#699=FACE_OUTER_BOUND('',#992,.T.);
#700=FACE_OUTER_BOUND('',#997,.T.);
#701=FACE_OUTER_BOUND('',#1002,.T.);
#702=FACE_OUTER_BOUND('',#1003,.T.);
#703=FACE_OUTER_BOUND('',#1004,.T.);
#704=FACE_OUTER_BOUND('',#1005,.T.);
#705=FACE_OUTER_BOUND('',#1006,.T.);
#706=FACE_OUTER_BOUND('',#1011,.T.);
#707=FACE_OUTER_BOUND('',#1012,.T.);
#708=FACE_OUTER_BOUND('',#1017,.T.);
#709=FACE_OUTER_BOUND('',#1018,.T.);
#710=FACE_OUTER_BOUND('',#1019,.T.);
#711=FACE_OUTER_BOUND('',#1020,.T.);
#712=FACE_OUTER_BOUND('',#1021,.T.);
#713=FACE_OUTER_BOUND('',#1022,.T.);
#714=FACE_OUTER_BOUND('',#1023,.T.);
#715=FACE_OUTER_BOUND('',#1024,.T.);
#716=FACE_OUTER_BOUND('',#1026,.T.);
#717=FACE_OUTER_BOUND('',#1027,.T.);
#718=FACE_OUTER_BOUND('',#1032,.T.);
#719=FACE_OUTER_BOUND('',#1033,.T.);
#720=FACE_OUTER_BOUND('',#1034,.T.);
#721=FACE_OUTER_BOUND('',#1035,.T.);
#722=FACE_OUTER_BOUND('',#1036,.T.);
#723=FACE_OUTER_BOUND('',#1041,.T.);
#724=FACE_OUTER_BOUND('',#1043,.T.);
#725=FACE_OUTER_BOUND('',#1044,.T.);
#726=FACE_OUTER_BOUND('',#1046,.T.);
#727=FACE_OUTER_BOUND('',#1047,.T.);
#728=FACE_OUTER_BOUND('',#1049,.T.);
#729=FACE_OUTER_BOUND('',#1050,.T.);
#730=FACE_OUTER_BOUND('',#1051,.T.);
#731=FACE_OUTER_BOUND('',#1052,.T.);
#732=FACE_OUTER_BOUND('',#1053,.T.);
#733=FACE_OUTER_BOUND('',#1054,.T.);
#734=FACE_OUTER_BOUND('',#1055,.T.);
#735=FACE_OUTER_BOUND('',#1057,.T.);
#736=FACE_OUTER_BOUND('',#1062,.T.);
#737=FACE_OUTER_BOUND('',#1063,.T.);
#738=FACE_OUTER_BOUND('',#1064,.T.);
#739=FACE_OUTER_BOUND('',#1065,.T.);
#740=FACE_OUTER_BOUND('',#1066,.T.);
#741=FACE_OUTER_BOUND('',#1068,.T.);
#742=FACE_OUTER_BOUND('',#1069,.T.);
#743=FACE_OUTER_BOUND('',#1074,.T.);
#744=FACE_OUTER_BOUND('',#1075,.T.);
#745=FACE_OUTER_BOUND('',#1076,.T.);
#746=FACE_OUTER_BOUND('',#1077,.T.);
#747=FACE_OUTER_BOUND('',#1078,.T.);
#748=FACE_OUTER_BOUND('',#1083,.T.);
#749=FACE_OUTER_BOUND('',#1084,.T.);
#750=FACE_OUTER_BOUND('',#1086,.T.);
#751=FACE_OUTER_BOUND('',#1087,.T.);
#752=FACE_OUTER_BOUND('',#1089,.T.);
#753=FACE_OUTER_BOUND('',#1090,.T.);
#754=FACE_OUTER_BOUND('',#1092,.T.);
#755=FACE_OUTER_BOUND('',#1094,.T.);
#756=FACE_OUTER_BOUND('',#1095,.T.);
#757=FACE_OUTER_BOUND('',#1096,.T.);
#758=FACE_OUTER_BOUND('',#1097,.T.);
#759=FACE_OUTER_BOUND('',#1098,.T.);
#760=FACE_OUTER_BOUND('',#1099,.T.);
#761=FACE_OUTER_BOUND('',#1104,.T.);
#762=FACE_OUTER_BOUND('',#1105,.T.);
#763=FACE_OUTER_BOUND('',#1106,.T.);
#764=FACE_OUTER_BOUND('',#1107,.T.);
#765=FACE_OUTER_BOUND('',#1108,.T.);
#766=FACE_OUTER_BOUND('',#1109,.T.);
#767=FACE_OUTER_BOUND('',#1110,.T.);
#768=FACE_OUTER_BOUND('',#1111,.T.);
#769=FACE_OUTER_BOUND('',#1112,.T.);
#770=FACE_OUTER_BOUND('',#1113,.T.);
#771=FACE_OUTER_BOUND('',#1115,.T.);
#772=FACE_OUTER_BOUND('',#1116,.T.);
#773=FACE_OUTER_BOUND('',#1118,.T.);
#774=FACE_OUTER_BOUND('',#1119,.T.);
#775=FACE_OUTER_BOUND('',#1120,.T.);
#776=FACE_OUTER_BOUND('',#1122,.T.);
#777=FACE_OUTER_BOUND('',#1123,.T.);
#778=FACE_OUTER_BOUND('',#1124,.T.);
#779=FACE_OUTER_BOUND('',#1125,.T.);
#780=FACE_OUTER_BOUND('',#1126,.T.);
#781=FACE_OUTER_BOUND('',#1128,.T.);
#782=FACE_OUTER_BOUND('',#1129,.T.);
#783=FACE_OUTER_BOUND('',#1131,.T.);
#784=FACE_OUTER_BOUND('',#1132,.T.);
#785=FACE_OUTER_BOUND('',#1133,.T.);
#786=FACE_OUTER_BOUND('',#1135,.T.);
#787=FACE_OUTER_BOUND('',#1136,.T.);
#788=FACE_OUTER_BOUND('',#1137,.T.);
#789=FACE_OUTER_BOUND('',#1139,.T.);
#790=FACE_OUTER_BOUND('',#1141,.T.);
#791=FACE_OUTER_BOUND('',#1142,.T.);
#792=FACE_OUTER_BOUND('',#1143,.T.);
#793=FACE_OUTER_BOUND('',#1144,.T.);
#794=FACE_OUTER_BOUND('',#1145,.T.);
#795=FACE_OUTER_BOUND('',#1146,.T.);
#796=FACE_OUTER_BOUND('',#1147,.T.);
#797=FACE_OUTER_BOUND('',#1148,.T.);
#798=FACE_OUTER_BOUND('',#1149,.T.);
#799=FACE_OUTER_BOUND('',#1150,.T.);
#800=FACE_OUTER_BOUND('',#1151,.T.);
#801=FACE_OUTER_BOUND('',#1152,.T.);
#802=FACE_OUTER_BOUND('',#1153,.T.);
#803=FACE_OUTER_BOUND('',#1154,.T.);
#804=FACE_OUTER_BOUND('',#1155,.T.);
#805=FACE_OUTER_BOUND('',#1156,.T.);
#806=FACE_OUTER_BOUND('',#1157,.T.);
#807=FACE_OUTER_BOUND('',#1158,.T.);
#808=FACE_OUTER_BOUND('',#1160,.T.);
#809=FACE_OUTER_BOUND('',#1162,.T.);
#810=FACE_OUTER_BOUND('',#1163,.T.);
#811=FACE_OUTER_BOUND('',#1164,.T.);
#812=FACE_OUTER_BOUND('',#1165,.T.);
#813=FACE_OUTER_BOUND('',#1166,.T.);
#814=FACE_OUTER_BOUND('',#1167,.T.);
#815=FACE_OUTER_BOUND('',#1168,.T.);
#816=FACE_OUTER_BOUND('',#1169,.T.);
#817=FACE_OUTER_BOUND('',#1170,.T.);
#818=FACE_OUTER_BOUND('',#1171,.T.);
#819=FACE_OUTER_BOUND('',#1172,.T.);
#820=FACE_OUTER_BOUND('',#1173,.T.);
#821=FACE_OUTER_BOUND('',#1174,.T.);
#822=FACE_OUTER_BOUND('',#1175,.T.);
#823=FACE_OUTER_BOUND('',#1177,.T.);
#824=FACE_OUTER_BOUND('',#1178,.T.);
#825=FACE_OUTER_BOUND('',#1179,.T.);
#826=FACE_OUTER_BOUND('',#1180,.T.);
#827=FACE_OUTER_BOUND('',#1181,.T.);
#828=FACE_OUTER_BOUND('',#1182,.T.);
#829=FACE_OUTER_BOUND('',#1183,.T.);
#830=FACE_OUTER_BOUND('',#1185,.T.);
#831=FACE_OUTER_BOUND('',#1186,.T.);
#832=FACE_OUTER_BOUND('',#1188,.T.);
#833=FACE_OUTER_BOUND('',#1189,.T.);
#834=FACE_OUTER_BOUND('',#1190,.T.);
#835=FACE_OUTER_BOUND('',#1191,.T.);
#836=FACE_OUTER_BOUND('',#1193,.T.);
#837=FACE_OUTER_BOUND('',#1194,.T.);
#838=FACE_OUTER_BOUND('',#1195,.T.);
#839=FACE_OUTER_BOUND('',#1196,.T.);
#840=FACE_OUTER_BOUND('',#1198,.T.);
#841=FACE_OUTER_BOUND('',#1199,.T.);
#842=FACE_OUTER_BOUND('',#1200,.T.);
#843=FACE_OUTER_BOUND('',#1201,.T.);
#844=FACE_OUTER_BOUND('',#1202,.T.);
#845=FACE_OUTER_BOUND('',#1203,.T.);
#846=FACE_OUTER_BOUND('',#1204,.T.);
#847=FACE_OUTER_BOUND('',#1205,.T.);
#848=FACE_OUTER_BOUND('',#1206,.T.);
#849=FACE_OUTER_BOUND('',#1207,.T.);
#850=FACE_OUTER_BOUND('',#1208,.T.);
#851=FACE_OUTER_BOUND('',#1209,.T.);
#852=FACE_OUTER_BOUND('',#1210,.T.);
#853=FACE_OUTER_BOUND('',#1211,.T.);
#854=FACE_OUTER_BOUND('',#1212,.T.);
#855=FACE_OUTER_BOUND('',#1213,.T.);
#856=FACE_OUTER_BOUND('',#1214,.T.);
#857=FACE_OUTER_BOUND('',#1215,.T.);
#858=FACE_OUTER_BOUND('',#1216,.T.);
#859=FACE_OUTER_BOUND('',#1217,.T.);
#860=FACE_OUTER_BOUND('',#1218,.T.);
#861=FACE_OUTER_BOUND('',#1219,.T.);
#862=FACE_OUTER_BOUND('',#1220,.T.);
#863=FACE_OUTER_BOUND('',#1221,.T.);
#864=FACE_OUTER_BOUND('',#1222,.T.);
#865=FACE_OUTER_BOUND('',#1223,.T.);
#866=FACE_OUTER_BOUND('',#1224,.T.);
#867=FACE_OUTER_BOUND('',#1226,.T.);
#868=FACE_OUTER_BOUND('',#1227,.T.);
#869=FACE_OUTER_BOUND('',#1229,.T.);
#870=FACE_OUTER_BOUND('',#1230,.T.);
#871=FACE_OUTER_BOUND('',#1232,.T.);
#872=FACE_OUTER_BOUND('',#1233,.T.);
#873=FACE_OUTER_BOUND('',#1235,.T.);
#874=FACE_OUTER_BOUND('',#1236,.T.);
#875=FACE_OUTER_BOUND('',#1238,.T.);
#876=FACE_OUTER_BOUND('',#1239,.T.);
#877=FACE_OUTER_BOUND('',#1240,.T.);
#878=FACE_OUTER_BOUND('',#1241,.T.);
#879=FACE_OUTER_BOUND('',#1242,.T.);
#880=FACE_OUTER_BOUND('',#1243,.T.);
#881=FACE_OUTER_BOUND('',#1244,.T.);
#882=FACE_OUTER_BOUND('',#1245,.T.);
#883=FACE_OUTER_BOUND('',#1246,.T.);
#884=FACE_OUTER_BOUND('',#1247,.T.);
#885=FACE_OUTER_BOUND('',#1248,.T.);
#886=FACE_OUTER_BOUND('',#1249,.T.);
#887=FACE_OUTER_BOUND('',#1250,.T.);
#888=FACE_OUTER_BOUND('',#1251,.T.);
#889=FACE_OUTER_BOUND('',#1252,.T.);
#890=FACE_OUTER_BOUND('',#1254,.T.);
#891=FACE_OUTER_BOUND('',#1255,.T.);
#892=FACE_OUTER_BOUND('',#1256,.T.);
#893=FACE_OUTER_BOUND('',#1257,.T.);
#894=FACE_OUTER_BOUND('',#1258,.T.);
#895=FACE_OUTER_BOUND('',#1259,.T.);
#896=FACE_OUTER_BOUND('',#1260,.T.);
#897=FACE_OUTER_BOUND('',#1261,.T.);
#898=FACE_OUTER_BOUND('',#1262,.T.);
#899=FACE_OUTER_BOUND('',#1264,.T.);
#900=FACE_OUTER_BOUND('',#1265,.T.);
#901=FACE_OUTER_BOUND('',#1270,.T.);
#902=FACE_OUTER_BOUND('',#1271,.T.);
#903=FACE_OUTER_BOUND('',#1272,.T.);
#904=FACE_OUTER_BOUND('',#1273,.T.);
#905=FACE_OUTER_BOUND('',#1274,.T.);
#906=FACE_OUTER_BOUND('',#1275,.T.);
#907=FACE_OUTER_BOUND('',#1280,.T.);
#908=FACE_OUTER_BOUND('',#1281,.T.);
#909=FACE_OUTER_BOUND('',#1282,.T.);
#910=FACE_OUTER_BOUND('',#1284,.T.);
#911=FACE_OUTER_BOUND('',#1286,.T.);
#912=FACE_OUTER_BOUND('',#1287,.T.);
#913=FACE_OUTER_BOUND('',#1288,.T.);
#914=FACE_OUTER_BOUND('',#1290,.T.);
#915=FACE_OUTER_BOUND('',#1292,.T.);
#916=FACE_OUTER_BOUND('',#1293,.T.);
#917=FACE_OUTER_BOUND('',#1294,.T.);
#918=FACE_OUTER_BOUND('',#1296,.T.);
#919=FACE_OUTER_BOUND('',#1298,.T.);
#920=FACE_OUTER_BOUND('',#1299,.T.);
#921=FACE_OUTER_BOUND('',#1300,.T.);
#922=FACE_OUTER_BOUND('',#1302,.T.);
#923=FACE_OUTER_BOUND('',#1304,.T.);
#924=FACE_OUTER_BOUND('',#1305,.T.);
#925=FACE_OUTER_BOUND('',#1306,.T.);
#926=FACE_OUTER_BOUND('',#1308,.T.);
#927=FACE_OUTER_BOUND('',#1310,.T.);
#928=FACE_OUTER_BOUND('',#1311,.T.);
#929=FACE_OUTER_BOUND('',#1312,.T.);
#930=FACE_OUTER_BOUND('',#1314,.T.);
#931=FACE_OUTER_BOUND('',#1316,.T.);
#932=FACE_OUTER_BOUND('',#1317,.T.);
#933=FACE_OUTER_BOUND('',#1318,.T.);
#934=FACE_OUTER_BOUND('',#1319,.T.);
#935=FACE_OUTER_BOUND('',#1320,.T.);
#936=FACE_OUTER_BOUND('',#1322,.T.);
#937=FACE_OUTER_BOUND('',#1323,.T.);
#938=FACE_OUTER_BOUND('',#1324,.T.);
#939=FACE_OUTER_BOUND('',#1325,.T.);
#940=FACE_OUTER_BOUND('',#1326,.T.);
#941=FACE_OUTER_BOUND('',#1327,.T.);
#942=FACE_OUTER_BOUND('',#1328,.T.);
#943=FACE_OUTER_BOUND('',#1329,.T.);
#944=FACE_OUTER_BOUND('',#1330,.T.);
#945=FACE_OUTER_BOUND('',#1331,.T.);
#946=FACE_OUTER_BOUND('',#1332,.T.);
#947=FACE_OUTER_BOUND('',#1333,.T.);
#948=EDGE_LOOP('',(#3207,#3208,#3209,#3210));
#949=EDGE_LOOP('',(#3211,#3212,#3213,#3214));
#950=EDGE_LOOP('',(#3215,#3216,#3217,#3218));
#951=EDGE_LOOP('',(#3219,#3220,#3221,#3222));
#952=EDGE_LOOP('',(#3223,#3224,#3225,#3226));
#953=EDGE_LOOP('',(#3227,#3228,#3229,#3230));
#954=EDGE_LOOP('',(#3231,#3232,#3233,#3234));
#955=EDGE_LOOP('',(#3235,#3236,#3237,#3238));
#956=EDGE_LOOP('',(#3239,#3240,#3241,#3242));
#957=EDGE_LOOP('',(#3243));
#958=EDGE_LOOP('',(#3244));
#959=EDGE_LOOP('',(#3245));
#960=EDGE_LOOP('',(#3246));
#961=EDGE_LOOP('',(#3247,#3248,#3249,#3250));
#962=EDGE_LOOP('',(#3251));
#963=EDGE_LOOP('',(#3252));
#964=EDGE_LOOP('',(#3253));
#965=EDGE_LOOP('',(#3254));
#966=EDGE_LOOP('',(#3255,#3256,#3257,#3258));
#967=EDGE_LOOP('',(#3259,#3260,#3261,#3262));
#968=EDGE_LOOP('',(#3263,#3264,#3265,#3266));
#969=EDGE_LOOP('',(#3267,#3268,#3269,#3270));
#970=EDGE_LOOP('',(#3271,#3272,#3273,#3274));
#971=EDGE_LOOP('',(#3275,#3276,#3277,#3278));
#972=EDGE_LOOP('',(#3279,#3280,#3281,#3282));
#973=EDGE_LOOP('',(#3283,#3284,#3285,#3286));
#974=EDGE_LOOP('',(#3287,#3288,#3289,#3290));
#975=EDGE_LOOP('',(#3291,#3292,#3293,#3294));
#976=EDGE_LOOP('',(#3295,#3296,#3297,#3298));
#977=EDGE_LOOP('',(#3299,#3300,#3301,#3302));
#978=EDGE_LOOP('',(#3303,#3304,#3305,#3306));
#979=EDGE_LOOP('',(#3307,#3308,#3309,#3310));
#980=EDGE_LOOP('',(#3311,#3312,#3313,#3314));
#981=EDGE_LOOP('',(#3315,#3316,#3317,#3318));
#982=EDGE_LOOP('',(#3319,#3320,#3321,#3322));
#983=EDGE_LOOP('',(#3323,#3324,#3325,#3326));
#984=EDGE_LOOP('',(#3327,#3328,#3329,#3330));
#985=EDGE_LOOP('',(#3331,#3332,#3333,#3334));
#986=EDGE_LOOP('',(#3335,#3336,#3337,#3338));
#987=EDGE_LOOP('',(#3339,#3340,#3341,#3342));
#988=EDGE_LOOP('',(#3343,#3344,#3345,#3346));
#989=EDGE_LOOP('',(#3347,#3348,#3349,#3350));
#990=EDGE_LOOP('',(#3351,#3352,#3353,#3354));
#991=EDGE_LOOP('',(#3355,#3356,#3357,#3358));
#992=EDGE_LOOP('',(#3359,#3360,#3361,#3362));
#993=EDGE_LOOP('',(#3363));
#994=EDGE_LOOP('',(#3364));
#995=EDGE_LOOP('',(#3365));
#996=EDGE_LOOP('',(#3366));
#997=EDGE_LOOP('',(#3367,#3368,#3369,#3370));
#998=EDGE_LOOP('',(#3371));
#999=EDGE_LOOP('',(#3372));
#1000=EDGE_LOOP('',(#3373));
#1001=EDGE_LOOP('',(#3374));
#1002=EDGE_LOOP('',(#3375,#3376,#3377,#3378));
#1003=EDGE_LOOP('',(#3379,#3380,#3381,#3382));
#1004=EDGE_LOOP('',(#3383,#3384,#3385,#3386));
#1005=EDGE_LOOP('',(#3387,#3388,#3389,#3390));
#1006=EDGE_LOOP('',(#3391,#3392,#3393,#3394));
#1007=EDGE_LOOP('',(#3395));
#1008=EDGE_LOOP('',(#3396));
#1009=EDGE_LOOP('',(#3397));
#1010=EDGE_LOOP('',(#3398));
#1011=EDGE_LOOP('',(#3399,#3400,#3401,#3402));
#1012=EDGE_LOOP('',(#3403,#3404,#3405,#3406));
#1013=EDGE_LOOP('',(#3407));
#1014=EDGE_LOOP('',(#3408));
#1015=EDGE_LOOP('',(#3409));
#1016=EDGE_LOOP('',(#3410));
#1017=EDGE_LOOP('',(#3411,#3412,#3413,#3414));
#1018=EDGE_LOOP('',(#3415,#3416,#3417,#3418));
#1019=EDGE_LOOP('',(#3419,#3420,#3421,#3422));
#1020=EDGE_LOOP('',(#3423,#3424,#3425,#3426));
#1021=EDGE_LOOP('',(#3427,#3428,#3429,#3430));
#1022=EDGE_LOOP('',(#3431,#3432,#3433,#3434));
#1023=EDGE_LOOP('',(#3435,#3436,#3437,#3438));
#1024=EDGE_LOOP('',(#3439));
#1025=EDGE_LOOP('',(#3440));
#1026=EDGE_LOOP('',(#3441,#3442,#3443,#3444));
#1027=EDGE_LOOP('',(#3445,#3446,#3447,#3448));
#1028=EDGE_LOOP('',(#3449));
#1029=EDGE_LOOP('',(#3450));
#1030=EDGE_LOOP('',(#3451));
#1031=EDGE_LOOP('',(#3452));
#1032=EDGE_LOOP('',(#3453,#3454,#3455,#3456));
#1033=EDGE_LOOP('',(#3457,#3458,#3459,#3460));
#1034=EDGE_LOOP('',(#3461,#3462,#3463,#3464));
#1035=EDGE_LOOP('',(#3465,#3466,#3467,#3468));
#1036=EDGE_LOOP('',(#3469,#3470,#3471,#3472));
#1037=EDGE_LOOP('',(#3473));
#1038=EDGE_LOOP('',(#3474));
#1039=EDGE_LOOP('',(#3475));
#1040=EDGE_LOOP('',(#3476));
#1041=EDGE_LOOP('',(#3477,#3478));
#1042=EDGE_LOOP('',(#3479));
#1043=EDGE_LOOP('',(#3480,#3481,#3482,#3483));
#1044=EDGE_LOOP('',(#3484,#3485));
#1045=EDGE_LOOP('',(#3486));
#1046=EDGE_LOOP('',(#3487,#3488,#3489,#3490));
#1047=EDGE_LOOP('',(#3491,#3492));
#1048=EDGE_LOOP('',(#3493));
#1049=EDGE_LOOP('',(#3494,#3495,#3496,#3497));
#1050=EDGE_LOOP('',(#3498,#3499,#3500,#3501,#3502,#3503,#3504,#3505,#3506,
#3507,#3508,#3509,#3510,#3511,#3512,#3513));
#1051=EDGE_LOOP('',(#3514,#3515,#3516,#3517));
#1052=EDGE_LOOP('',(#3518,#3519,#3520,#3521));
#1053=EDGE_LOOP('',(#3522,#3523,#3524,#3525));
#1054=EDGE_LOOP('',(#3526,#3527,#3528,#3529));
#1055=EDGE_LOOP('',(#3530,#3531,#3532,#3533,#3534,#3535,#3536));
#1056=EDGE_LOOP('',(#3537));
#1057=EDGE_LOOP('',(#3538));
#1058=EDGE_LOOP('',(#3539));
#1059=EDGE_LOOP('',(#3540));
#1060=EDGE_LOOP('',(#3541));
#1061=EDGE_LOOP('',(#3542));
#1062=EDGE_LOOP('',(#3543,#3544,#3545,#3546));
#1063=EDGE_LOOP('',(#3547,#3548,#3549,#3550));
#1064=EDGE_LOOP('',(#3551,#3552,#3553,#3554));
#1065=EDGE_LOOP('',(#3555,#3556,#3557,#3558));
#1066=EDGE_LOOP('',(#3559));
#1067=EDGE_LOOP('',(#3560));
#1068=EDGE_LOOP('',(#3561,#3562,#3563,#3564));
#1069=EDGE_LOOP('',(#3565,#3566,#3567,#3568));
#1070=EDGE_LOOP('',(#3569));
#1071=EDGE_LOOP('',(#3570));
#1072=EDGE_LOOP('',(#3571));
#1073=EDGE_LOOP('',(#3572));
#1074=EDGE_LOOP('',(#3573,#3574,#3575,#3576));
#1075=EDGE_LOOP('',(#3577,#3578,#3579,#3580));
#1076=EDGE_LOOP('',(#3581,#3582,#3583,#3584));
#1077=EDGE_LOOP('',(#3585,#3586,#3587,#3588));
#1078=EDGE_LOOP('',(#3589,#3590,#3591,#3592));
#1079=EDGE_LOOP('',(#3593));
#1080=EDGE_LOOP('',(#3594));
#1081=EDGE_LOOP('',(#3595));
#1082=EDGE_LOOP('',(#3596));
#1083=EDGE_LOOP('',(#3597,#3598,#3599,#3600));
#1084=EDGE_LOOP('',(#3601,#3602));
#1085=EDGE_LOOP('',(#3603));
#1086=EDGE_LOOP('',(#3604,#3605,#3606,#3607));
#1087=EDGE_LOOP('',(#3608,#3609));
#1088=EDGE_LOOP('',(#3610));
#1089=EDGE_LOOP('',(#3611,#3612,#3613,#3614));
#1090=EDGE_LOOP('',(#3615,#3616));
#1091=EDGE_LOOP('',(#3617));
#1092=EDGE_LOOP('',(#3618,#3619,#3620,#3621,#3622,#3623,#3624));
#1093=EDGE_LOOP('',(#3625));
#1094=EDGE_LOOP('',(#3626,#3627,#3628,#3629));
#1095=EDGE_LOOP('',(#3630,#3631,#3632,#3633));
#1096=EDGE_LOOP('',(#3634,#3635,#3636,#3637));
#1097=EDGE_LOOP('',(#3638,#3639,#3640,#3641));
#1098=EDGE_LOOP('',(#3642,#3643,#3644,#3645,#3646,#3647,#3648,#3649,#3650,
#3651,#3652,#3653,#3654,#3655,#3656,#3657));
#1099=EDGE_LOOP('',(#3658));
#1100=EDGE_LOOP('',(#3659));
#1101=EDGE_LOOP('',(#3660));
#1102=EDGE_LOOP('',(#3661));
#1103=EDGE_LOOP('',(#3662));
#1104=EDGE_LOOP('',(#3663,#3664,#3665,#3666));
#1105=EDGE_LOOP('',(#3667,#3668,#3669,#3670));
#1106=EDGE_LOOP('',(#3671,#3672,#3673,#3674));
#1107=EDGE_LOOP('',(#3675,#3676,#3677,#3678,#3679,#3680,#3681,#3682,#3683,
#3684));
#1108=EDGE_LOOP('',(#3685,#3686,#3687,#3688));
#1109=EDGE_LOOP('',(#3689,#3690,#3691,#3692));
#1110=EDGE_LOOP('',(#3693,#3694,#3695,#3696));
#1111=EDGE_LOOP('',(#3697,#3698,#3699,#3700));
#1112=EDGE_LOOP('',(#3701,#3702,#3703,#3704));
#1113=EDGE_LOOP('',(#3705,#3706,#3707,#3708));
#1114=EDGE_LOOP('',(#3709));
#1115=EDGE_LOOP('',(#3710,#3711,#3712,#3713));
#1116=EDGE_LOOP('',(#3714,#3715,#3716,#3717));
#1117=EDGE_LOOP('',(#3718));
#1118=EDGE_LOOP('',(#3719,#3720,#3721,#3722,#3723,#3724,#3725,#3726,#3727,
#3728));
#1119=EDGE_LOOP('',(#3729,#3730));
#1120=EDGE_LOOP('',(#3731));
#1121=EDGE_LOOP('',(#3732));
#1122=EDGE_LOOP('',(#3733,#3734,#3735,#3736));
#1123=EDGE_LOOP('',(#3737,#3738,#3739,#3740));
#1124=EDGE_LOOP('',(#3741));
#1125=EDGE_LOOP('',(#3742));
#1126=EDGE_LOOP('',(#3743));
#1127=EDGE_LOOP('',(#3744));
#1128=EDGE_LOOP('',(#3745,#3746,#3747,#3748));
#1129=EDGE_LOOP('',(#3749));
#1130=EDGE_LOOP('',(#3750));
#1131=EDGE_LOOP('',(#3751,#3752,#3753,#3754));
#1132=EDGE_LOOP('',(#3755,#3756,#3757,#3758));
#1133=EDGE_LOOP('',(#3759));
#1134=EDGE_LOOP('',(#3760));
#1135=EDGE_LOOP('',(#3761,#3762,#3763,#3764));
#1136=EDGE_LOOP('',(#3765,#3766,#3767,#3768));
#1137=EDGE_LOOP('',(#3769));
#1138=EDGE_LOOP('',(#3770));
#1139=EDGE_LOOP('',(#3771));
#1140=EDGE_LOOP('',(#3772));
#1141=EDGE_LOOP('',(#3773,#3774,#3775,#3776));
#1142=EDGE_LOOP('',(#3777));
#1143=EDGE_LOOP('',(#3778));
#1144=EDGE_LOOP('',(#3779,#3780,#3781,#3782));
#1145=EDGE_LOOP('',(#3783,#3784,#3785,#3786));
#1146=EDGE_LOOP('',(#3787,#3788,#3789,#3790));
#1147=EDGE_LOOP('',(#3791,#3792,#3793,#3794));
#1148=EDGE_LOOP('',(#3795,#3796,#3797,#3798));
#1149=EDGE_LOOP('',(#3799,#3800,#3801,#3802));
#1150=EDGE_LOOP('',(#3803,#3804,#3805,#3806));
#1151=EDGE_LOOP('',(#3807,#3808,#3809,#3810));
#1152=EDGE_LOOP('',(#3811,#3812,#3813,#3814));
#1153=EDGE_LOOP('',(#3815,#3816,#3817,#3818));
#1154=EDGE_LOOP('',(#3819,#3820,#3821,#3822));
#1155=EDGE_LOOP('',(#3823,#3824,#3825,#3826));
#1156=EDGE_LOOP('',(#3827,#3828,#3829,#3830));
#1157=EDGE_LOOP('',(#3831,#3832,#3833,#3834));
#1158=EDGE_LOOP('',(#3835));
#1159=EDGE_LOOP('',(#3836));
#1160=EDGE_LOOP('',(#3837));
#1161=EDGE_LOOP('',(#3838));
#1162=EDGE_LOOP('',(#3839,#3840,#3841,#3842));
#1163=EDGE_LOOP('',(#3843,#3844,#3845,#3846));
#1164=EDGE_LOOP('',(#3847,#3848,#3849,#3850));
#1165=EDGE_LOOP('',(#3851,#3852,#3853,#3854));
#1166=EDGE_LOOP('',(#3855,#3856,#3857,#3858));
#1167=EDGE_LOOP('',(#3859,#3860,#3861,#3862));
#1168=EDGE_LOOP('',(#3863,#3864,#3865,#3866,#3867,#3868));
#1169=EDGE_LOOP('',(#3869,#3870,#3871,#3872,#3873,#3874));
#1170=EDGE_LOOP('',(#3875));
#1171=EDGE_LOOP('',(#3876));
#1172=EDGE_LOOP('',(#3877,#3878,#3879,#3880));
#1173=EDGE_LOOP('',(#3881,#3882,#3883,#3884));
#1174=EDGE_LOOP('',(#3885,#3886,#3887,#3888));
#1175=EDGE_LOOP('',(#3889));
#1176=EDGE_LOOP('',(#3890));
#1177=EDGE_LOOP('',(#3891,#3892,#3893,#3894));
#1178=EDGE_LOOP('',(#3895,#3896,#3897,#3898));
#1179=EDGE_LOOP('',(#3899,#3900,#3901,#3902,#3903,#3904));
#1180=EDGE_LOOP('',(#3905,#3906,#3907,#3908,#3909));
#1181=EDGE_LOOP('',(#3910,#3911,#3912,#3913));
#1182=EDGE_LOOP('',(#3914,#3915,#3916,#3917));
#1183=EDGE_LOOP('',(#3918));
#1184=EDGE_LOOP('',(#3919));
#1185=EDGE_LOOP('',(#3920,#3921,#3922,#3923,#3924));
#1186=EDGE_LOOP('',(#3925));
#1187=EDGE_LOOP('',(#3926));
#1188=EDGE_LOOP('',(#3927,#3928,#3929,#3930));
#1189=EDGE_LOOP('',(#3931,#3932,#3933,#3934,#3935,#3936));
#1190=EDGE_LOOP('',(#3937,#3938,#3939,#3940,#3941));
#1191=EDGE_LOOP('',(#3942));
#1192=EDGE_LOOP('',(#3943));
#1193=EDGE_LOOP('',(#3944,#3945,#3946,#3947));
#1194=EDGE_LOOP('',(#3948,#3949,#3950,#3951));
#1195=EDGE_LOOP('',(#3952,#3953,#3954,#3955));
#1196=EDGE_LOOP('',(#3956));
#1197=EDGE_LOOP('',(#3957));
#1198=EDGE_LOOP('',(#3958,#3959,#3960,#3961,#3962));
#1199=EDGE_LOOP('',(#3963,#3964));
#1200=EDGE_LOOP('',(#3965,#3966));
#1201=EDGE_LOOP('',(#3967,#3968));
#1202=EDGE_LOOP('',(#3969,#3970));
#1203=EDGE_LOOP('',(#3971,#3972));
#1204=EDGE_LOOP('',(#3973,#3974));
#1205=EDGE_LOOP('',(#3975,#3976));
#1206=EDGE_LOOP('',(#3977,#3978));
#1207=EDGE_LOOP('',(#3979,#3980,#3981,#3982));
#1208=EDGE_LOOP('',(#3983,#3984,#3985,#3986,#3987,#3988,#3989,#3990,#3991,
#3992,#3993,#3994,#3995,#3996,#3997,#3998,#3999,#4000,#4001,#4002));
#1209=EDGE_LOOP('',(#4003,#4004,#4005,#4006));
#1210=EDGE_LOOP('',(#4007,#4008,#4009,#4010));
#1211=EDGE_LOOP('',(#4011,#4012,#4013,#4014));
#1212=EDGE_LOOP('',(#4015,#4016,#4017,#4018));
#1213=EDGE_LOOP('',(#4019,#4020,#4021,#4022));
#1214=EDGE_LOOP('',(#4023,#4024,#4025,#4026,#4027,#4028));
#1215=EDGE_LOOP('',(#4029,#4030,#4031,#4032));
#1216=EDGE_LOOP('',(#4033,#4034,#4035,#4036));
#1217=EDGE_LOOP('',(#4037,#4038,#4039,#4040));
#1218=EDGE_LOOP('',(#4041,#4042,#4043,#4044));
#1219=EDGE_LOOP('',(#4045,#4046,#4047,#4048));
#1220=EDGE_LOOP('',(#4049,#4050,#4051,#4052));
#1221=EDGE_LOOP('',(#4053,#4054,#4055,#4056,#4057,#4058,#4059,#4060,#4061,
#4062,#4063,#4064,#4065,#4066,#4067,#4068,#4069,#4070,#4071,#4072));
#1222=EDGE_LOOP('',(#4073,#4074,#4075,#4076));
#1223=EDGE_LOOP('',(#4077,#4078,#4079,#4080));
#1224=EDGE_LOOP('',(#4081));
#1225=EDGE_LOOP('',(#4082));
#1226=EDGE_LOOP('',(#4083,#4084,#4085,#4086));
#1227=EDGE_LOOP('',(#4087));
#1228=EDGE_LOOP('',(#4088));
#1229=EDGE_LOOP('',(#4089,#4090,#4091,#4092));
#1230=EDGE_LOOP('',(#4093));
#1231=EDGE_LOOP('',(#4094));
#1232=EDGE_LOOP('',(#4095,#4096,#4097,#4098));
#1233=EDGE_LOOP('',(#4099));
#1234=EDGE_LOOP('',(#4100));
#1235=EDGE_LOOP('',(#4101,#4102,#4103,#4104));
#1236=EDGE_LOOP('',(#4105));
#1237=EDGE_LOOP('',(#4106));
#1238=EDGE_LOOP('',(#4107,#4108,#4109,#4110));
#1239=EDGE_LOOP('',(#4111,#4112,#4113,#4114));
#1240=EDGE_LOOP('',(#4115,#4116,#4117,#4118));
#1241=EDGE_LOOP('',(#4119,#4120,#4121,#4122));
#1242=EDGE_LOOP('',(#4123,#4124,#4125,#4126));
#1243=EDGE_LOOP('',(#4127,#4128,#4129,#4130));
#1244=EDGE_LOOP('',(#4131,#4132,#4133,#4134));
#1245=EDGE_LOOP('',(#4135,#4136,#4137,#4138,#4139,#4140));
#1246=EDGE_LOOP('',(#4141,#4142,#4143,#4144,#4145,#4146));
#1247=EDGE_LOOP('',(#4147));
#1248=EDGE_LOOP('',(#4148));
#1249=EDGE_LOOP('',(#4149,#4150,#4151,#4152));
#1250=EDGE_LOOP('',(#4153,#4154,#4155,#4156));
#1251=EDGE_LOOP('',(#4157,#4158,#4159,#4160));
#1252=EDGE_LOOP('',(#4161));
#1253=EDGE_LOOP('',(#4162));
#1254=EDGE_LOOP('',(#4163,#4164,#4165,#4166));
#1255=EDGE_LOOP('',(#4167,#4168,#4169,#4170));
#1256=EDGE_LOOP('',(#4171,#4172,#4173,#4174));
#1257=EDGE_LOOP('',(#4175));
#1258=EDGE_LOOP('',(#4176,#4177,#4178,#4179));
#1259=EDGE_LOOP('',(#4180));
#1260=EDGE_LOOP('',(#4181));
#1261=EDGE_LOOP('',(#4182,#4183,#4184,#4185));
#1262=EDGE_LOOP('',(#4186,#4187,#4188,#4189));
#1263=EDGE_LOOP('',(#4190));
#1264=EDGE_LOOP('',(#4191,#4192,#4193,#4194));
#1265=EDGE_LOOP('',(#4195,#4196,#4197,#4198,#4199,#4200,#4201,#4202));
#1266=EDGE_LOOP('',(#4203));
#1267=EDGE_LOOP('',(#4204));
#1268=EDGE_LOOP('',(#4205));
#1269=EDGE_LOOP('',(#4206));
#1270=EDGE_LOOP('',(#4207,#4208,#4209,#4210));
#1271=EDGE_LOOP('',(#4211,#4212,#4213,#4214));
#1272=EDGE_LOOP('',(#4215,#4216,#4217,#4218));
#1273=EDGE_LOOP('',(#4219,#4220,#4221,#4222));
#1274=EDGE_LOOP('',(#4223,#4224,#4225,#4226));
#1275=EDGE_LOOP('',(#4227,#4228,#4229,#4230,#4231,#4232,#4233,#4234));
#1276=EDGE_LOOP('',(#4235));
#1277=EDGE_LOOP('',(#4236));
#1278=EDGE_LOOP('',(#4237));
#1279=EDGE_LOOP('',(#4238));
#1280=EDGE_LOOP('',(#4239,#4240,#4241,#4242));
#1281=EDGE_LOOP('',(#4243,#4244,#4245,#4246));
#1282=EDGE_LOOP('',(#4247,#4248,#4249,#4250));
#1283=EDGE_LOOP('',(#4251));
#1284=EDGE_LOOP('',(#4252,#4253,#4254,#4255));
#1285=EDGE_LOOP('',(#4256));
#1286=EDGE_LOOP('',(#4257,#4258,#4259,#4260));
#1287=EDGE_LOOP('',(#4261,#4262,#4263,#4264));
#1288=EDGE_LOOP('',(#4265));
#1289=EDGE_LOOP('',(#4266));
#1290=EDGE_LOOP('',(#4267));
#1291=EDGE_LOOP('',(#4268));
#1292=EDGE_LOOP('',(#4269,#4270,#4271,#4272));
#1293=EDGE_LOOP('',(#4273,#4274,#4275,#4276));
#1294=EDGE_LOOP('',(#4277));
#1295=EDGE_LOOP('',(#4278));
#1296=EDGE_LOOP('',(#4279));
#1297=EDGE_LOOP('',(#4280));
#1298=EDGE_LOOP('',(#4281,#4282,#4283,#4284));
#1299=EDGE_LOOP('',(#4285,#4286,#4287,#4288));
#1300=EDGE_LOOP('',(#4289));
#1301=EDGE_LOOP('',(#4290));
#1302=EDGE_LOOP('',(#4291));
#1303=EDGE_LOOP('',(#4292));
#1304=EDGE_LOOP('',(#4293,#4294,#4295,#4296));
#1305=EDGE_LOOP('',(#4297,#4298,#4299,#4300));
#1306=EDGE_LOOP('',(#4301));
#1307=EDGE_LOOP('',(#4302));
#1308=EDGE_LOOP('',(#4303));
#1309=EDGE_LOOP('',(#4304));
#1310=EDGE_LOOP('',(#4305,#4306,#4307,#4308));
#1311=EDGE_LOOP('',(#4309,#4310,#4311,#4312));
#1312=EDGE_LOOP('',(#4313));
#1313=EDGE_LOOP('',(#4314));
#1314=EDGE_LOOP('',(#4315));
#1315=EDGE_LOOP('',(#4316));
#1316=EDGE_LOOP('',(#4317));
#1317=EDGE_LOOP('',(#4318,#4319,#4320,#4321));
#1318=EDGE_LOOP('',(#4322,#4323,#4324,#4325));
#1319=EDGE_LOOP('',(#4326,#4327,#4328,#4329));
#1320=EDGE_LOOP('',(#4330));
#1321=EDGE_LOOP('',(#4331));
#1322=EDGE_LOOP('',(#4332,#4333,#4334,#4335));
#1323=EDGE_LOOP('',(#4336,#4337,#4338,#4339));
#1324=EDGE_LOOP('',(#4340,#4341,#4342,#4343));
#1325=EDGE_LOOP('',(#4344));
#1326=EDGE_LOOP('',(#4345,#4346,#4347,#4348));
#1327=EDGE_LOOP('',(#4349,#4350,#4351,#4352));
#1328=EDGE_LOOP('',(#4353,#4354,#4355,#4356));
#1329=EDGE_LOOP('',(#4357,#4358,#4359,#4360));
#1330=EDGE_LOOP('',(#4361,#4362,#4363,#4364));
#1331=EDGE_LOOP('',(#4365,#4366,#4367,#4368));
#1332=EDGE_LOOP('',(#4369,#4370,#4371,#4372,#4373,#4374));
#1333=EDGE_LOOP('',(#4375,#4376,#4377,#4378,#4379,#4380));
#1334=LINE('',#7304,#1654);
#1335=LINE('',#7310,#1655);
#1336=LINE('',#7316,#1656);
#1337=LINE('',#7322,#1657);
#1338=LINE('',#7327,#1658);
#1339=LINE('',#7329,#1659);
#1340=LINE('',#7331,#1660);
#1341=LINE('',#7332,#1661);
#1342=LINE('',#7335,#1662);
#1343=LINE('',#7337,#1663);
#1344=LINE('',#7338,#1664);
#1345=LINE('',#7341,#1665);
#1346=LINE('',#7343,#1666);
#1347=LINE('',#7344,#1667);
#1348=LINE('',#7346,#1668);
#1349=LINE('',#7347,#1669);
#1350=LINE('',#7354,#1670);
#1351=LINE('',#7356,#1671);
#1352=LINE('',#7358,#1672);
#1353=LINE('',#7359,#1673);
#1354=LINE('',#7362,#1674);
#1355=LINE('',#7364,#1675);
#1356=LINE('',#7365,#1676);
#1357=LINE('',#7368,#1677);
#1358=LINE('',#7370,#1678);
#1359=LINE('',#7371,#1679);
#1360=LINE('',#7373,#1680);
#1361=LINE('',#7374,#1681);
#1362=LINE('',#7381,#1682);
#1363=LINE('',#7383,#1683);
#1364=LINE('',#7385,#1684);
#1365=LINE('',#7386,#1685);
#1366=LINE('',#7389,#1686);
#1367=LINE('',#7391,#1687);
#1368=LINE('',#7392,#1688);
#1369=LINE('',#7395,#1689);
#1370=LINE('',#7397,#1690);
#1371=LINE('',#7398,#1691);
#1372=LINE('',#7400,#1692);
#1373=LINE('',#7401,#1693);
#1374=LINE('',#7408,#1694);
#1375=LINE('',#7410,#1695);
#1376=LINE('',#7412,#1696);
#1377=LINE('',#7413,#1697);
#1378=LINE('',#7416,#1698);
#1379=LINE('',#7418,#1699);
#1380=LINE('',#7419,#1700);
#1381=LINE('',#7422,#1701);
#1382=LINE('',#7424,#1702);
#1383=LINE('',#7425,#1703);
#1384=LINE('',#7427,#1704);
#1385=LINE('',#7428,#1705);
#1386=LINE('',#7435,#1706);
#1387=LINE('',#7441,#1707);
#1388=LINE('',#7447,#1708);
#1389=LINE('',#7453,#1709);
#1390=LINE('',#7458,#1710);
#1391=LINE('',#7460,#1711);
#1392=LINE('',#7462,#1712);
#1393=LINE('',#7463,#1713);
#1394=LINE('',#7466,#1714);
#1395=LINE('',#7468,#1715);
#1396=LINE('',#7469,#1716);
#1397=LINE('',#7472,#1717);
#1398=LINE('',#7474,#1718);
#1399=LINE('',#7475,#1719);
#1400=LINE('',#7477,#1720);
#1401=LINE('',#7478,#1721);
#1402=LINE('',#7486,#1722);
#1403=LINE('',#7492,#1723);
#1404=LINE('',#7498,#1724);
#1405=LINE('',#7504,#1725);
#1406=LINE('',#7509,#1726);
#1407=LINE('',#7511,#1727);
#1408=LINE('',#7513,#1728);
#1409=LINE('',#7514,#1729);
#1410=LINE('',#7517,#1730);
#1411=LINE('',#7519,#1731);
#1412=LINE('',#7520,#1732);
#1413=LINE('',#7523,#1733);
#1414=LINE('',#7525,#1734);
#1415=LINE('',#7526,#1735);
#1416=LINE('',#7528,#1736);
#1417=LINE('',#7529,#1737);
#1418=LINE('',#7537,#1738);
#1419=LINE('',#7543,#1739);
#1420=LINE('',#7549,#1740);
#1421=LINE('',#7555,#1741);
#1422=LINE('',#7563,#1742);
#1423=LINE('',#7567,#1743);
#1424=LINE('',#7569,#1744);
#1425=LINE('',#7571,#1745);
#1426=LINE('',#7575,#1746);
#1427=LINE('',#7577,#1747);
#1428=LINE('',#7578,#1748);
#1429=LINE('',#7581,#1749);
#1430=LINE('',#7583,#1750);
#1431=LINE('',#7584,#1751);
#1432=LINE('',#7586,#1752);
#1433=LINE('',#7600,#1753);
#1434=LINE('',#7603,#1754);
#1435=LINE('',#7613,#1755);
#1436=LINE('',#7616,#1756);
#1437=LINE('',#7626,#1757);
#1438=LINE('',#7629,#1758);
#1439=LINE('',#7635,#1759);
#1440=LINE('',#7642,#1760);
#1441=LINE('',#7646,#1761);
#1442=LINE('',#7650,#1762);
#1443=LINE('',#7655,#1763);
#1444=LINE('',#7664,#1764);
#1445=LINE('',#7670,#1765);
#1446=LINE('',#7676,#1766);
#1447=LINE('',#7682,#1767);
#1448=LINE('',#7689,#1768);
#1449=LINE('',#7694,#1769);
#1450=LINE('',#7696,#1770);
#1451=LINE('',#7698,#1771);
#1452=LINE('',#7702,#1772);
#1453=LINE('',#7704,#1773);
#1454=LINE('',#7705,#1774);
#1455=LINE('',#7708,#1775);
#1456=LINE('',#7710,#1776);
#1457=LINE('',#7711,#1777);
#1458=LINE('',#7713,#1778);
#1459=LINE('',#7721,#1779);
#1460=LINE('',#7725,#1780);
#1461=LINE('',#7734,#1781);
#1462=LINE('',#7738,#1782);
#1463=LINE('',#7747,#1783);
#1464=LINE('',#7751,#1784);
#1465=LINE('',#7767,#1785);
#1466=LINE('',#7771,#1786);
#1467=LINE('',#7775,#1787);
#1468=LINE('',#7780,#1788);
#1469=LINE('',#7784,#1789);
#1470=LINE('',#7791,#1790);
#1471=LINE('',#7796,#1791);
#1472=LINE('',#7798,#1792);
#1473=LINE('',#7800,#1793);
#1474=LINE('',#7801,#1794);
#1475=LINE('',#7804,#1795);
#1476=LINE('',#7806,#1796);
#1477=LINE('',#7807,#1797);
#1478=LINE('',#7811,#1798);
#1479=LINE('',#7813,#1799);
#1480=LINE('',#7815,#1800);
#1481=LINE('',#7817,#1801);
#1482=LINE('',#7819,#1802);
#1483=LINE('',#7821,#1803);
#1484=LINE('',#7822,#1804);
#1485=LINE('',#7823,#1805);
#1486=LINE('',#7826,#1806);
#1487=LINE('',#7827,#1807);
#1488=LINE('',#7830,#1808);
#1489=LINE('',#7831,#1809);
#1490=LINE('',#7834,#1810);
#1491=LINE('',#7835,#1811);
#1492=LINE('',#7838,#1812);
#1493=LINE('',#7839,#1813);
#1494=LINE('',#7842,#1814);
#1495=LINE('',#7843,#1815);
#1496=LINE('',#7846,#1816);
#1497=LINE('',#7847,#1817);
#1498=LINE('',#7850,#1818);
#1499=LINE('',#7851,#1819);
#1500=LINE('',#7853,#1820);
#1501=LINE('',#7869,#1821);
#1502=LINE('',#7872,#1822);
#1503=LINE('',#7884,#1823);
#1504=LINE('',#7892,#1824);
#1505=LINE('',#7896,#1825);
#1506=LINE('',#7903,#1826);
#1507=LINE('',#7909,#1827);
#1508=LINE('',#8639,#1828);
#1509=LINE('',#8641,#1829);
#1510=LINE('',#8643,#1830);
#1511=LINE('',#8644,#1831);
#1512=LINE('',#8647,#1832);
#1513=LINE('',#8649,#1833);
#1514=LINE('',#8650,#1834);
#1515=LINE('',#8653,#1835);
#1516=LINE('',#8655,#1836);
#1517=LINE('',#8656,#1837);
#1518=LINE('',#8658,#1838);
#1519=LINE('',#8659,#1839);
#1520=LINE('',#8666,#1840);
#1521=LINE('',#8668,#1841);
#1522=LINE('',#8670,#1842);
#1523=LINE('',#8671,#1843);
#1524=LINE('',#8674,#1844);
#1525=LINE('',#8676,#1845);
#1526=LINE('',#8677,#1846);
#1527=LINE('',#8680,#1847);
#1528=LINE('',#8682,#1848);
#1529=LINE('',#8683,#1849);
#1530=LINE('',#8685,#1850);
#1531=LINE('',#8686,#1851);
#1532=LINE('',#8694,#1852);
#1533=LINE('',#8700,#1853);
#1534=LINE('',#8708,#1854);
#1535=LINE('',#8710,#1855);
#1536=LINE('',#8712,#1856);
#1537=LINE('',#8713,#1857);
#1538=LINE('',#8716,#1858);
#1539=LINE('',#8718,#1859);
#1540=LINE('',#8719,#1860);
#1541=LINE('',#8722,#1861);
#1542=LINE('',#8724,#1862);
#1543=LINE('',#8725,#1863);
#1544=LINE('',#8728,#1864);
#1545=LINE('',#8730,#1865);
#1546=LINE('',#8731,#1866);
#1547=LINE('',#8734,#1867);
#1548=LINE('',#8736,#1868);
#1549=LINE('',#8737,#1869);
#1550=LINE('',#8739,#1870);
#1551=LINE('',#8740,#1871);
#1552=LINE('',#8752,#1872);
#1553=LINE('',#8756,#1873);
#1554=LINE('',#8760,#1874);
#1555=LINE('',#8767,#1875);
#1556=LINE('',#8769,#1876);
#1557=LINE('',#8784,#1877);
#1558=LINE('',#8790,#1878);
#1559=LINE('',#8794,#1879);
#1560=LINE('',#8800,#1880);
#1561=LINE('',#8805,#1881);
#1562=LINE('',#8820,#1882);
#1563=LINE('',#8829,#1883);
#1564=LINE('',#8833,#1884);
#1565=LINE('',#8837,#1885);
#1566=LINE('',#8840,#1886);
#1567=LINE('',#8993,#1887);
#1568=LINE('',#9289,#1888);
#1569=LINE('',#9331,#1889);
#1570=LINE('',#9336,#1890);
#1571=LINE('',#9345,#1891);
#1572=LINE('',#9350,#1892);
#1573=LINE('',#9360,#1893);
#1574=LINE('',#9362,#1894);
#1575=LINE('',#9364,#1895);
#1576=LINE('',#9365,#1896);
#1577=LINE('',#9368,#1897);
#1578=LINE('',#9370,#1898);
#1579=LINE('',#9371,#1899);
#1580=LINE('',#9374,#1900);
#1581=LINE('',#9376,#1901);
#1582=LINE('',#9377,#1902);
#1583=LINE('',#9380,#1903);
#1584=LINE('',#9382,#1904);
#1585=LINE('',#9383,#1905);
#1586=LINE('',#9386,#1906);
#1587=LINE('',#9388,#1907);
#1588=LINE('',#9389,#1908);
#1589=LINE('',#9391,#1909);
#1590=LINE('',#9392,#1910);
#1591=LINE('',#9404,#1911);
#1592=LINE('',#9408,#1912);
#1593=LINE('',#9412,#1913);
#1594=LINE('',#9419,#1914);
#1595=LINE('',#9421,#1915);
#1596=LINE('',#9461,#1916);
#1597=LINE('',#9468,#1917);
#1598=LINE('',#9518,#1918);
#1599=LINE('',#9522,#1919);
#1600=LINE('',#9526,#1920);
#1601=LINE('',#9528,#1921);
#1602=LINE('',#9532,#1922);
#1603=LINE('',#9534,#1923);
#1604=LINE('',#9538,#1924);
#1605=LINE('',#9540,#1925);
#1606=LINE('',#9542,#1926);
#1607=LINE('',#9544,#1927);
#1608=LINE('',#9545,#1928);
#1609=LINE('',#9556,#1929);
#1610=LINE('',#9560,#1930);
#1611=LINE('',#9564,#1931);
#1612=LINE('',#9568,#1932);
#1613=LINE('',#9572,#1933);
#1614=LINE('',#9576,#1934);
#1615=LINE('',#9578,#1935);
#1616=LINE('',#9580,#1936);
#1617=LINE('',#9581,#1937);
#1618=LINE('',#9583,#1938);
#1619=LINE('',#9584,#1939);
#1620=LINE('',#9595,#1940);
#1621=LINE('',#9600,#1941);
#1622=LINE('',#9608,#1942);
#1623=LINE('',#9614,#1943);
#1624=LINE('',#9623,#1944);
#1625=LINE('',#9629,#1945);
#1626=LINE('',#9638,#1946);
#1627=LINE('',#9644,#1947);
#1628=LINE('',#9653,#1948);
#1629=LINE('',#9659,#1949);
#1630=LINE('',#9670,#1950);
#1631=LINE('',#9674,#1951);
#1632=LINE('',#9678,#1952);
#1633=LINE('',#9685,#1953);
#1634=LINE('',#9689,#1954);
#1635=LINE('',#9693,#1955);
#1636=LINE('',#9698,#1956);
#1637=LINE('',#9700,#1957);
#1638=LINE('',#9702,#1958);
#1639=LINE('',#9703,#1959);
#1640=LINE('',#9706,#1960);
#1641=LINE('',#9708,#1961);
#1642=LINE('',#9709,#1962);
#1643=LINE('',#9712,#1963);
#1644=LINE('',#9714,#1964);
#1645=LINE('',#9715,#1965);
#1646=LINE('',#9718,#1966);
#1647=LINE('',#9720,#1967);
#1648=LINE('',#9721,#1968);
#1649=LINE('',#9724,#1969);
#1650=LINE('',#9726,#1970);
#1651=LINE('',#9727,#1971);
#1652=LINE('',#9729,#1972);
#1653=LINE('',#9730,#1973);
#1654=VECTOR('',#5761,0.25);
#1655=VECTOR('',#5768,0.25);
#1656=VECTOR('',#5775,0.25);
#1657=VECTOR('',#5782,0.25);
#1658=VECTOR('',#5787,1.);
#1659=VECTOR('',#5788,1.);
#1660=VECTOR('',#5789,1.);
#1661=VECTOR('',#5790,1.);
#1662=VECTOR('',#5793,1.);
#1663=VECTOR('',#5794,1.);
#1664=VECTOR('',#5795,1.);
#1665=VECTOR('',#5798,1.);
#1666=VECTOR('',#5799,1.);
#1667=VECTOR('',#5800,1.);
#1668=VECTOR('',#5803,1.);
#1669=VECTOR('',#5804,1.);
#1670=VECTOR('',#5813,1.);
#1671=VECTOR('',#5814,1.);
#1672=VECTOR('',#5815,1.);
#1673=VECTOR('',#5816,1.);
#1674=VECTOR('',#5819,1.);
#1675=VECTOR('',#5820,1.);
#1676=VECTOR('',#5821,1.);
#1677=VECTOR('',#5824,1.);
#1678=VECTOR('',#5825,1.);
#1679=VECTOR('',#5826,1.);
#1680=VECTOR('',#5829,1.);
#1681=VECTOR('',#5830,1.);
#1682=VECTOR('',#5839,1.);
#1683=VECTOR('',#5840,1.);
#1684=VECTOR('',#5841,1.);
#1685=VECTOR('',#5842,1.);
#1686=VECTOR('',#5845,1.);
#1687=VECTOR('',#5846,1.);
#1688=VECTOR('',#5847,1.);
#1689=VECTOR('',#5850,1.);
#1690=VECTOR('',#5851,1.);
#1691=VECTOR('',#5852,1.);
#1692=VECTOR('',#5855,1.);
#1693=VECTOR('',#5856,1.);
#1694=VECTOR('',#5865,1.);
#1695=VECTOR('',#5866,1.);
#1696=VECTOR('',#5867,1.);
#1697=VECTOR('',#5868,1.);
#1698=VECTOR('',#5871,1.);
#1699=VECTOR('',#5872,1.);
#1700=VECTOR('',#5873,1.);
#1701=VECTOR('',#5876,1.);
#1702=VECTOR('',#5877,1.);
#1703=VECTOR('',#5878,1.);
#1704=VECTOR('',#5881,1.);
#1705=VECTOR('',#5882,1.);
#1706=VECTOR('',#5891,0.33);
#1707=VECTOR('',#5898,0.33);
#1708=VECTOR('',#5905,0.33);
#1709=VECTOR('',#5912,0.33);
#1710=VECTOR('',#5917,1.);
#1711=VECTOR('',#5918,1.);
#1712=VECTOR('',#5919,1.);
#1713=VECTOR('',#5920,1.);
#1714=VECTOR('',#5923,1.);
#1715=VECTOR('',#5924,1.);
#1716=VECTOR('',#5925,1.);
#1717=VECTOR('',#5928,1.);
#1718=VECTOR('',#5929,1.);
#1719=VECTOR('',#5930,1.);
#1720=VECTOR('',#5933,1.);
#1721=VECTOR('',#5934,1.);
#1722=VECTOR('',#5945,0.33);
#1723=VECTOR('',#5952,0.33);
#1724=VECTOR('',#5959,0.33);
#1725=VECTOR('',#5966,0.33);
#1726=VECTOR('',#5971,1.);
#1727=VECTOR('',#5972,1.);
#1728=VECTOR('',#5973,1.);
#1729=VECTOR('',#5974,1.);
#1730=VECTOR('',#5977,1.);
#1731=VECTOR('',#5978,1.);
#1732=VECTOR('',#5979,1.);
#1733=VECTOR('',#5982,1.);
#1734=VECTOR('',#5983,1.);
#1735=VECTOR('',#5984,1.);
#1736=VECTOR('',#5987,1.);
#1737=VECTOR('',#5988,1.);
#1738=VECTOR('',#5999,0.165);
#1739=VECTOR('',#6006,0.165);
#1740=VECTOR('',#6013,0.165);
#1741=VECTOR('',#6020,1.5);
#1742=VECTOR('',#6031,1.02);
#1743=VECTOR('',#6034,1.);
#1744=VECTOR('',#6035,1.);
#1745=VECTOR('',#6036,1.);
#1746=VECTOR('',#6041,1.);
#1747=VECTOR('',#6042,1.);
#1748=VECTOR('',#6043,1.);
#1749=VECTOR('',#6046,1.);
#1750=VECTOR('',#6047,1.);
#1751=VECTOR('',#6048,1.);
#1752=VECTOR('',#6051,1.);
#1753=VECTOR('',#6070,1.);
#1754=VECTOR('',#6073,1.);
#1755=VECTOR('',#6084,1.);
#1756=VECTOR('',#6087,1.);
#1757=VECTOR('',#6098,1.);
#1758=VECTOR('',#6101,1.);
#1759=VECTOR('',#6108,2.1);
#1760=VECTOR('',#6119,0.225);
#1761=VECTOR('',#6124,0.225);
#1762=VECTOR('',#6129,0.225);
#1763=VECTOR('',#6134,1.02);
#1764=VECTOR('',#6147,0.165);
#1765=VECTOR('',#6154,0.165);
#1766=VECTOR('',#6161,0.165);
#1767=VECTOR('',#6168,1.5);
#1768=VECTOR('',#6177,1.02);
#1769=VECTOR('',#6182,1.);
#1770=VECTOR('',#6183,1.);
#1771=VECTOR('',#6184,1.);
#1772=VECTOR('',#6189,1.);
#1773=VECTOR('',#6190,1.);
#1774=VECTOR('',#6191,1.);
#1775=VECTOR('',#6194,1.);
#1776=VECTOR('',#6195,1.);
#1777=VECTOR('',#6196,1.);
#1778=VECTOR('',#6199,1.);
#1779=VECTOR('',#6210,1.);
#1780=VECTOR('',#6213,1.);
#1781=VECTOR('',#6224,1.);
#1782=VECTOR('',#6227,1.);
#1783=VECTOR('',#6238,1.);
#1784=VECTOR('',#6241,1.);
#1785=VECTOR('',#6264,0.225);
#1786=VECTOR('',#6269,0.225);
#1787=VECTOR('',#6274,0.225);
#1788=VECTOR('',#6281,1.02);
#1789=VECTOR('',#6286,2.1);
#1790=VECTOR('',#6295,0.31);
#1791=VECTOR('',#6300,1.);
#1792=VECTOR('',#6301,1.);
#1793=VECTOR('',#6302,1.);
#1794=VECTOR('',#6303,1.);
#1795=VECTOR('',#6306,1.);
#1796=VECTOR('',#6307,1.);
#1797=VECTOR('',#6308,1.);
#1798=VECTOR('',#6311,1.);
#1799=VECTOR('',#6312,1.);
#1800=VECTOR('',#6313,1.);
#1801=VECTOR('',#6314,1.);
#1802=VECTOR('',#6315,1.);
#1803=VECTOR('',#6316,1.);
#1804=VECTOR('',#6317,1.);
#1805=VECTOR('',#6318,1.);
#1806=VECTOR('',#6321,1.);
#1807=VECTOR('',#6322,1.);
#1808=VECTOR('',#6325,1.);
#1809=VECTOR('',#6326,1.);
#1810=VECTOR('',#6329,1.);
#1811=VECTOR('',#6330,1.);
#1812=VECTOR('',#6333,1.);
#1813=VECTOR('',#6334,1.);
#1814=VECTOR('',#6337,1.);
#1815=VECTOR('',#6338,1.);
#1816=VECTOR('',#6341,1.);
#1817=VECTOR('',#6342,1.);
#1818=VECTOR('',#6345,1.);
#1819=VECTOR('',#6346,1.);
#1820=VECTOR('',#6349,1.);
#1821=VECTOR('',#6370,0.29);
#1822=VECTOR('',#6373,0.1);
#1823=VECTOR('',#6390,0.6);
#1824=VECTOR('',#6401,0.11);
#1825=VECTOR('',#6406,0.31);
#1826=VECTOR('',#6415,0.1);
#1827=VECTOR('',#6422,0.6);
#1828=VECTOR('',#6443,1.);
#1829=VECTOR('',#6444,1.);
#1830=VECTOR('',#6445,1.);
#1831=VECTOR('',#6446,1.);
#1832=VECTOR('',#6449,1.);
#1833=VECTOR('',#6450,1.);
#1834=VECTOR('',#6451,1.);
#1835=VECTOR('',#6454,1.);
#1836=VECTOR('',#6455,1.);
#1837=VECTOR('',#6456,1.);
#1838=VECTOR('',#6459,1.);
#1839=VECTOR('',#6460,1.);
#1840=VECTOR('',#6469,1.);
#1841=VECTOR('',#6470,1.);
#1842=VECTOR('',#6471,1.);
#1843=VECTOR('',#6472,1.);
#1844=VECTOR('',#6475,1.);
#1845=VECTOR('',#6476,1.);
#1846=VECTOR('',#6477,1.);
#1847=VECTOR('',#6480,1.);
#1848=VECTOR('',#6481,1.);
#1849=VECTOR('',#6482,1.);
#1850=VECTOR('',#6485,1.);
#1851=VECTOR('',#6486,1.);
#1852=VECTOR('',#6497,0.32);
#1853=VECTOR('',#6504,0.6);
#1854=VECTOR('',#6515,1.);
#1855=VECTOR('',#6516,1.);
#1856=VECTOR('',#6517,1.);
#1857=VECTOR('',#6518,1.);
#1858=VECTOR('',#6521,1.);
#1859=VECTOR('',#6522,1.);
#1860=VECTOR('',#6523,1.);
#1861=VECTOR('',#6526,1.);
#1862=VECTOR('',#6527,1.);
#1863=VECTOR('',#6528,1.);
#1864=VECTOR('',#6531,1.);
#1865=VECTOR('',#6532,1.);
#1866=VECTOR('',#6533,1.);
#1867=VECTOR('',#6536,1.);
#1868=VECTOR('',#6537,1.);
#1869=VECTOR('',#6538,1.);
#1870=VECTOR('',#6541,1.);
#1871=VECTOR('',#6542,1.);
#1872=VECTOR('',#6559,0.475);
#1873=VECTOR('',#6564,0.5);
#1874=VECTOR('',#6569,0.485);
#1875=VECTOR('',#6578,0.31);
#1876=VECTOR('',#6581,0.3);
#1877=VECTOR('',#6600,0.976185);
#1878=VECTOR('',#6607,0.5);
#1879=VECTOR('',#6612,0.53);
#1880=VECTOR('',#6621,0.976185);
#1881=VECTOR('',#6628,0.53);
#1882=VECTOR('',#6647,1.023815);
#1883=VECTOR('',#6658,1.47);
#1884=VECTOR('',#6663,1.5);
#1885=VECTOR('',#6668,1.47);
#1886=VECTOR('',#6673,1.023815);
#1887=VECTOR('',#6724,1.019052);
#1888=VECTOR('',#6801,0.980948);
#1889=VECTOR('',#6830,1.013815);
#1890=VECTOR('',#6837,0.991185);
#1891=VECTOR('',#6848,1.013815);
#1892=VECTOR('',#6855,0.991185);
#1893=VECTOR('',#6870,1.);
#1894=VECTOR('',#6871,1.);
#1895=VECTOR('',#6872,1.);
#1896=VECTOR('',#6873,1.);
#1897=VECTOR('',#6876,1.);
#1898=VECTOR('',#6877,1.);
#1899=VECTOR('',#6878,1.);
#1900=VECTOR('',#6881,1.);
#1901=VECTOR('',#6882,1.);
#1902=VECTOR('',#6883,1.);
#1903=VECTOR('',#6886,1.);
#1904=VECTOR('',#6887,1.);
#1905=VECTOR('',#6888,1.);
#1906=VECTOR('',#6891,1.);
#1907=VECTOR('',#6892,1.);
#1908=VECTOR('',#6893,1.);
#1909=VECTOR('',#6896,1.);
#1910=VECTOR('',#6897,1.);
#1911=VECTOR('',#6914,0.325);
#1912=VECTOR('',#6919,0.35);
#1913=VECTOR('',#6924,0.335);
#1914=VECTOR('',#6933,0.21);
#1915=VECTOR('',#6936,0.2);
#1916=VECTOR('',#7011,0.165);
#1917=VECTOR('',#7020,0.165);
#1918=VECTOR('',#7029,1.);
#1919=VECTOR('',#7032,1.);
#1920=VECTOR('',#7037,1.);
#1921=VECTOR('',#7038,1.);
#1922=VECTOR('',#7043,1.);
#1923=VECTOR('',#7044,1.);
#1924=VECTOR('',#7049,1.);
#1925=VECTOR('',#7050,1.);
#1926=VECTOR('',#7051,1.);
#1927=VECTOR('',#7052,1.);
#1928=VECTOR('',#7053,1.);
#1929=VECTOR('',#7064,1.);
#1930=VECTOR('',#7069,0.33);
#1931=VECTOR('',#7074,0.33);
#1932=VECTOR('',#7079,0.33);
#1933=VECTOR('',#7084,0.33);
#1934=VECTOR('',#7089,1.);
#1935=VECTOR('',#7090,1.);
#1936=VECTOR('',#7091,1.);
#1937=VECTOR('',#7092,1.);
#1938=VECTOR('',#7095,1.);
#1939=VECTOR('',#7096,1.);
#1940=VECTOR('',#7111,0.5);
#1941=VECTOR('',#7118,0.5);
#1942=VECTOR('',#7129,0.505);
#1943=VECTOR('',#7136,0.7);
#1944=VECTOR('',#7149,0.505);
#1945=VECTOR('',#7156,0.7);
#1946=VECTOR('',#7169,0.225);
#1947=VECTOR('',#7176,0.9);
#1948=VECTOR('',#7189,0.225);
#1949=VECTOR('',#7196,0.9);
#1950=VECTOR('',#7213,0.325);
#1951=VECTOR('',#7218,0.35);
#1952=VECTOR('',#7223,0.335);
#1953=VECTOR('',#7232,0.21);
#1954=VECTOR('',#7237,0.2);
#1955=VECTOR('',#7242,0.18);
#1956=VECTOR('',#7247,1.);
#1957=VECTOR('',#7248,1.);
#1958=VECTOR('',#7249,1.);
#1959=VECTOR('',#7250,1.);
#1960=VECTOR('',#7253,1.);
#1961=VECTOR('',#7254,1.);
#1962=VECTOR('',#7255,1.);
#1963=VECTOR('',#7258,1.);
#1964=VECTOR('',#7259,1.);
#1965=VECTOR('',#7260,1.);
#1966=VECTOR('',#7263,1.);
#1967=VECTOR('',#7264,1.);
#1968=VECTOR('',#7265,1.);
#1969=VECTOR('',#7268,1.);
#1970=VECTOR('',#7269,1.);
#1971=VECTOR('',#7270,1.);
#1972=VECTOR('',#7273,1.);
#1973=VECTOR('',#7274,1.);
#1974=CIRCLE('',#5142,0.25);
#1975=CIRCLE('',#5143,0.25);
#1976=CIRCLE('',#5145,0.25);
#1977=CIRCLE('',#5146,0.25);
#1978=CIRCLE('',#5148,0.25);
#1979=CIRCLE('',#5149,0.25);
#1980=CIRCLE('',#5151,0.25);
#1981=CIRCLE('',#5152,0.25);
#1982=CIRCLE('',#5181,0.33);
#1983=CIRCLE('',#5182,0.33);
#1984=CIRCLE('',#5184,0.33);
#1985=CIRCLE('',#5185,0.33);
#1986=CIRCLE('',#5187,0.33);
#1987=CIRCLE('',#5188,0.33);
#1988=CIRCLE('',#5190,0.33);
#1989=CIRCLE('',#5191,0.33);
#1990=CIRCLE('',#5200,0.33);
#1991=CIRCLE('',#5201,0.33);
#1992=CIRCLE('',#5203,0.33);
#1993=CIRCLE('',#5204,0.33);
#1994=CIRCLE('',#5206,0.33);
#1995=CIRCLE('',#5207,0.33);
#1996=CIRCLE('',#5209,0.33);
#1997=CIRCLE('',#5210,0.33);
#1998=CIRCLE('',#5219,0.165);
#1999=CIRCLE('',#5220,0.165);
#2000=CIRCLE('',#5222,0.165);
#2001=CIRCLE('',#5223,0.165);
#2002=CIRCLE('',#5225,0.165);
#2003=CIRCLE('',#5226,0.165);
#2004=CIRCLE('',#5228,1.5);
#2005=CIRCLE('',#5229,1.5);
#2006=CIRCLE('',#5231,1.02);
#2007=CIRCLE('',#5233,1.02);
#2008=CIRCLE('',#5235,2.1);
#2009=CIRCLE('',#5240,2.1);
#2010=CIRCLE('',#5244,2.1);
#2011=CIRCLE('',#5245,0.375);
#2012=CIRCLE('',#5246,0.225);
#2013=CIRCLE('',#5248,0.375);
#2014=CIRCLE('',#5250,2.1);
#2015=CIRCLE('',#5251,0.375);
#2016=CIRCLE('',#5252,0.225);
#2017=CIRCLE('',#5254,0.375);
#2018=CIRCLE('',#5256,2.1);
#2019=CIRCLE('',#5257,0.375);
#2020=CIRCLE('',#5258,0.225);
#2021=CIRCLE('',#5260,0.375);
#2022=CIRCLE('',#5262,2.1);
#2023=CIRCLE('',#5263,2.1);
#2024=CIRCLE('',#5264,2.1);
#2025=CIRCLE('',#5265,2.1);
#2026=CIRCLE('',#5266,2.1);
#2027=CIRCLE('',#5268,0.225);
#2028=CIRCLE('',#5270,0.225);
#2029=CIRCLE('',#5272,0.225);
#2030=CIRCLE('',#5274,1.02);
#2031=CIRCLE('',#5275,1.02);
#2032=CIRCLE('',#5280,0.165);
#2033=CIRCLE('',#5281,0.165);
#2034=CIRCLE('',#5283,0.165);
#2035=CIRCLE('',#5284,0.165);
#2036=CIRCLE('',#5286,0.165);
#2037=CIRCLE('',#5287,0.165);
#2038=CIRCLE('',#5289,1.5);
#2039=CIRCLE('',#5290,1.5);
#2040=CIRCLE('',#5292,1.02);
#2041=CIRCLE('',#5294,1.02);
#2042=CIRCLE('',#5296,2.1);
#2043=CIRCLE('',#5301,2.1);
#2044=CIRCLE('',#5305,0.375);
#2045=CIRCLE('',#5306,0.375);
#2046=CIRCLE('',#5308,2.1);
#2047=CIRCLE('',#5309,0.225);
#2048=CIRCLE('',#5311,0.375);
#2049=CIRCLE('',#5312,0.375);
#2050=CIRCLE('',#5314,2.1);
#2051=CIRCLE('',#5315,0.225);
#2052=CIRCLE('',#5317,0.375);
#2053=CIRCLE('',#5318,0.375);
#2054=CIRCLE('',#5320,2.1);
#2055=CIRCLE('',#5321,0.225);
#2056=CIRCLE('',#5323,2.1);
#2057=CIRCLE('',#5324,2.1);
#2058=CIRCLE('',#5325,2.1);
#2059=CIRCLE('',#5326,2.1);
#2060=CIRCLE('',#5327,1.02);
#2061=CIRCLE('',#5329,0.225);
#2062=CIRCLE('',#5331,0.225);
#2063=CIRCLE('',#5333,0.225);
#2064=CIRCLE('',#5335,1.02);
#2065=CIRCLE('',#5337,2.1);
#2066=CIRCLE('',#5341,0.31);
#2067=CIRCLE('',#5342,0.31);
#2068=CIRCLE('',#5357,0.3);
#2069=CIRCLE('',#5360,0.29);
#2070=CIRCLE('',#5361,0.1);
#2071=CIRCLE('',#5363,0.29);
#2072=CIRCLE('',#5365,0.1);
#2073=CIRCLE('',#5370,0.6);
#2074=CIRCLE('',#5371,0.31);
#2075=CIRCLE('',#5373,0.6);
#2076=CIRCLE('',#5375,0.11);
#2077=CIRCLE('',#5377,0.11);
#2078=CIRCLE('',#5379,0.31);
#2079=CIRCLE('',#5383,0.1);
#2080=CIRCLE('',#5384,0.1);
#2081=CIRCLE('',#5386,0.6);
#2082=CIRCLE('',#5387,0.6);
#2083=CIRCLE('',#5391,0.03);
#2084=CIRCLE('',#5392,0.03);
#2085=CIRCLE('',#5411,0.32);
#2086=CIRCLE('',#5412,0.32);
#2087=CIRCLE('',#5414,0.6);
#2088=CIRCLE('',#5415,0.6);
#2089=CIRCLE('',#5428,0.2942);
#2090=CIRCLE('',#5430,0.45);
#2091=CIRCLE('',#5432,0.5);
#2092=CIRCLE('',#5434,0.5);
#2093=CIRCLE('',#5436,0.47);
#2094=CIRCLE('',#5438,0.32);
#2095=CIRCLE('',#5440,0.2942);
#2096=CIRCLE('',#5445,0.976185);
#2097=CIRCLE('',#5446,0.976185);
#2098=CIRCLE('',#5447,0.247676);
#2099=CIRCLE('',#5448,0.976185);
#2100=CIRCLE('',#5449,0.976185);
#2101=CIRCLE('',#5451,0.976185);
#2102=CIRCLE('',#5453,0.5);
#2103=CIRCLE('',#5454,0.5);
#2104=CIRCLE('',#5456,0.56);
#2105=CIRCLE('',#5459,0.976185);
#2106=CIRCLE('',#5461,0.56);
#2107=CIRCLE('',#5465,1.023815);
#2108=CIRCLE('',#5466,1.023815);
#2109=CIRCLE('',#5467,0.247676);
#2110=CIRCLE('',#5468,1.023815);
#2111=CIRCLE('',#5469,1.023815);
#2112=CIRCLE('',#5471,1.023815);
#2113=CIRCLE('',#5473,1.44);
#2114=CIRCLE('',#5474,1.023815);
#2115=CIRCLE('',#5476,1.5);
#2116=CIRCLE('',#5478,1.5);
#2117=CIRCLE('',#5480,1.44);
#2118=CIRCLE('',#5485,0.23815);
#2119=CIRCLE('',#5487,0.23815);
#2120=CIRCLE('',#5489,0.23815);
#2121=CIRCLE('',#5491,0.23815);
#2122=CIRCLE('',#5493,0.23815);
#2123=CIRCLE('',#5495,0.23815);
#2124=CIRCLE('',#5497,0.23815);
#2125=CIRCLE('',#5499,0.23815);
#2126=CIRCLE('',#5502,0.243053047864041);
#2127=CIRCLE('',#5503,0.243053047864041);
#2128=CIRCLE('',#5505,1.019052);
#2129=CIRCLE('',#5506,1.019052);
#2130=CIRCLE('',#5507,1.019052);
#2131=CIRCLE('',#5508,1.019052);
#2132=CIRCLE('',#5509,1.019052);
#2133=CIRCLE('',#5510,1.019052);
#2134=CIRCLE('',#5511,1.019052);
#2135=CIRCLE('',#5512,1.019052);
#2136=CIRCLE('',#5513,1.019052);
#2137=CIRCLE('',#5515,0.980948);
#2138=CIRCLE('',#5516,0.243053047864041);
#2139=CIRCLE('',#5518,0.243053047864041);
#2140=CIRCLE('',#5520,0.980948);
#2141=CIRCLE('',#5521,0.243053047864041);
#2142=CIRCLE('',#5523,0.243053047864041);
#2143=CIRCLE('',#5525,0.980948);
#2144=CIRCLE('',#5526,0.243053047864041);
#2145=CIRCLE('',#5528,0.243053047864041);
#2146=CIRCLE('',#5530,0.980948);
#2147=CIRCLE('',#5531,0.243053047864041);
#2148=CIRCLE('',#5533,0.243053047864041);
#2149=CIRCLE('',#5535,0.980948);
#2150=CIRCLE('',#5536,0.243053047864041);
#2151=CIRCLE('',#5538,0.243053047864041);
#2152=CIRCLE('',#5540,0.980948);
#2153=CIRCLE('',#5541,0.243053047864041);
#2154=CIRCLE('',#5543,0.243053047864041);
#2155=CIRCLE('',#5545,0.980948);
#2156=CIRCLE('',#5546,0.980948);
#2157=CIRCLE('',#5547,0.980948);
#2158=CIRCLE('',#5549,0.243053047864041);
#2159=CIRCLE('',#5551,0.243053047864041);
#2160=CIRCLE('',#5556,1.013815);
#2161=CIRCLE('',#5557,0.991185);
#2162=CIRCLE('',#5559,1.013815);
#2163=CIRCLE('',#5561,0.991185);
#2164=CIRCLE('',#5564,1.013815);
#2165=CIRCLE('',#5565,0.991185);
#2166=CIRCLE('',#5567,1.013815);
#2167=CIRCLE('',#5569,0.991185);
#2168=CIRCLE('',#5586,0.1954);
#2169=CIRCLE('',#5588,0.3);
#2170=CIRCLE('',#5590,0.35);
#2171=CIRCLE('',#5592,0.35);
#2172=CIRCLE('',#5594,0.32);
#2173=CIRCLE('',#5596,0.22);
#2174=CIRCLE('',#5598,0.1954);
#2175=CIRCLE('',#5636,0.165);
#2176=CIRCLE('',#5637,0.165);
#2177=CIRCLE('',#5640,0.165);
#2178=CIRCLE('',#5641,0.165);
#2179=CIRCLE('',#5645,1.);
#2180=CIRCLE('',#5646,1.8);
#2181=CIRCLE('',#5648,1.8);
#2182=CIRCLE('',#5650,1.);
#2183=CIRCLE('',#5652,0.33);
#2184=CIRCLE('',#5653,0.33);
#2185=CIRCLE('',#5654,0.33);
#2186=CIRCLE('',#5655,0.33);
#2187=CIRCLE('',#5657,1.);
#2188=CIRCLE('',#5659,0.33);
#2189=CIRCLE('',#5661,0.33);
#2190=CIRCLE('',#5663,0.33);
#2191=CIRCLE('',#5665,0.33);
#2192=CIRCLE('',#5669,1.);
#2193=CIRCLE('',#5671,0.5);
#2194=CIRCLE('',#5673,0.5);
#2195=CIRCLE('',#5675,0.5);
#2196=CIRCLE('',#5677,0.5);
#2197=CIRCLE('',#5682,0.505);
#2198=CIRCLE('',#5683,0.505);
#2199=CIRCLE('',#5685,0.7);
#2200=CIRCLE('',#5686,0.7);
#2201=CIRCLE('',#5691,0.505);
#2202=CIRCLE('',#5692,0.505);
#2203=CIRCLE('',#5694,0.7);
#2204=CIRCLE('',#5695,0.7);
#2205=CIRCLE('',#5700,0.225);
#2206=CIRCLE('',#5701,0.225);
#2207=CIRCLE('',#5703,0.9);
#2208=CIRCLE('',#5704,0.9);
#2209=CIRCLE('',#5709,0.225);
#2210=CIRCLE('',#5710,0.225);
#2211=CIRCLE('',#5712,0.9);
#2212=CIRCLE('',#5713,0.9);
#2213=CIRCLE('',#5718,0.3);
#2214=CIRCLE('',#5720,0.35);
#2215=CIRCLE('',#5722,0.35);
#2216=CIRCLE('',#5724,0.32);
#2217=CIRCLE('',#5726,0.22);
#2218=CIRCLE('',#5728,0.1954);
#2219=CIRCLE('',#5730,0.1954);
#2220=CIRCLE('',#5732,0.16);
#2221=VERTEX_POINT('',#7301);
#2222=VERTEX_POINT('',#7303);
#2223=VERTEX_POINT('',#7307);
#2224=VERTEX_POINT('',#7309);
#2225=VERTEX_POINT('',#7313);
#2226=VERTEX_POINT('',#7315);
#2227=VERTEX_POINT('',#7319);
#2228=VERTEX_POINT('',#7321);
#2229=VERTEX_POINT('',#7325);
#2230=VERTEX_POINT('',#7326);
#2231=VERTEX_POINT('',#7328);
#2232=VERTEX_POINT('',#7330);
#2233=VERTEX_POINT('',#7334);
#2234=VERTEX_POINT('',#7336);
#2235=VERTEX_POINT('',#7340);
#2236=VERTEX_POINT('',#7342);
#2237=VERTEX_POINT('',#7352);
#2238=VERTEX_POINT('',#7353);
#2239=VERTEX_POINT('',#7355);
#2240=VERTEX_POINT('',#7357);
#2241=VERTEX_POINT('',#7361);
#2242=VERTEX_POINT('',#7363);
#2243=VERTEX_POINT('',#7367);
#2244=VERTEX_POINT('',#7369);
#2245=VERTEX_POINT('',#7379);
#2246=VERTEX_POINT('',#7380);
#2247=VERTEX_POINT('',#7382);
#2248=VERTEX_POINT('',#7384);
#2249=VERTEX_POINT('',#7388);
#2250=VERTEX_POINT('',#7390);
#2251=VERTEX_POINT('',#7394);
#2252=VERTEX_POINT('',#7396);
#2253=VERTEX_POINT('',#7406);
#2254=VERTEX_POINT('',#7407);
#2255=VERTEX_POINT('',#7409);
#2256=VERTEX_POINT('',#7411);
#2257=VERTEX_POINT('',#7415);
#2258=VERTEX_POINT('',#7417);
#2259=VERTEX_POINT('',#7421);
#2260=VERTEX_POINT('',#7423);
#2261=VERTEX_POINT('',#7432);
#2262=VERTEX_POINT('',#7434);
#2263=VERTEX_POINT('',#7438);
#2264=VERTEX_POINT('',#7440);
#2265=VERTEX_POINT('',#7444);
#2266=VERTEX_POINT('',#7446);
#2267=VERTEX_POINT('',#7450);
#2268=VERTEX_POINT('',#7452);
#2269=VERTEX_POINT('',#7456);
#2270=VERTEX_POINT('',#7457);
#2271=VERTEX_POINT('',#7459);
#2272=VERTEX_POINT('',#7461);
#2273=VERTEX_POINT('',#7465);
#2274=VERTEX_POINT('',#7467);
#2275=VERTEX_POINT('',#7471);
#2276=VERTEX_POINT('',#7473);
#2277=VERTEX_POINT('',#7483);
#2278=VERTEX_POINT('',#7485);
#2279=VERTEX_POINT('',#7489);
#2280=VERTEX_POINT('',#7491);
#2281=VERTEX_POINT('',#7495);
#2282=VERTEX_POINT('',#7497);
#2283=VERTEX_POINT('',#7501);
#2284=VERTEX_POINT('',#7503);
#2285=VERTEX_POINT('',#7507);
#2286=VERTEX_POINT('',#7508);
#2287=VERTEX_POINT('',#7510);
#2288=VERTEX_POINT('',#7512);
#2289=VERTEX_POINT('',#7516);
#2290=VERTEX_POINT('',#7518);
#2291=VERTEX_POINT('',#7522);
#2292=VERTEX_POINT('',#7524);
#2293=VERTEX_POINT('',#7534);
#2294=VERTEX_POINT('',#7536);
#2295=VERTEX_POINT('',#7540);
#2296=VERTEX_POINT('',#7542);
#2297=VERTEX_POINT('',#7546);
#2298=VERTEX_POINT('',#7548);
#2299=VERTEX_POINT('',#7552);
#2300=VERTEX_POINT('',#7554);
#2301=VERTEX_POINT('',#7558);
#2302=VERTEX_POINT('',#7561);
#2303=VERTEX_POINT('',#7565);
#2304=VERTEX_POINT('',#7566);
#2305=VERTEX_POINT('',#7568);
#2306=VERTEX_POINT('',#7570);
#2307=VERTEX_POINT('',#7574);
#2308=VERTEX_POINT('',#7576);
#2309=VERTEX_POINT('',#7580);
#2310=VERTEX_POINT('',#7582);
#2311=VERTEX_POINT('',#7592);
#2312=VERTEX_POINT('',#7593);
#2313=VERTEX_POINT('',#7596);
#2314=VERTEX_POINT('',#7599);
#2315=VERTEX_POINT('',#7601);
#2316=VERTEX_POINT('',#7605);
#2317=VERTEX_POINT('',#7606);
#2318=VERTEX_POINT('',#7609);
#2319=VERTEX_POINT('',#7612);
#2320=VERTEX_POINT('',#7614);
#2321=VERTEX_POINT('',#7618);
#2322=VERTEX_POINT('',#7619);
#2323=VERTEX_POINT('',#7622);
#2324=VERTEX_POINT('',#7625);
#2325=VERTEX_POINT('',#7627);
#2326=VERTEX_POINT('',#7632);
#2327=VERTEX_POINT('',#7634);
#2328=VERTEX_POINT('',#7640);
#2329=VERTEX_POINT('',#7644);
#2330=VERTEX_POINT('',#7648);
#2331=VERTEX_POINT('',#7652);
#2332=VERTEX_POINT('',#7654);
#2333=VERTEX_POINT('',#7661);
#2334=VERTEX_POINT('',#7663);
#2335=VERTEX_POINT('',#7667);
#2336=VERTEX_POINT('',#7669);
#2337=VERTEX_POINT('',#7673);
#2338=VERTEX_POINT('',#7675);
#2339=VERTEX_POINT('',#7679);
#2340=VERTEX_POINT('',#7681);
#2341=VERTEX_POINT('',#7685);
#2342=VERTEX_POINT('',#7688);
#2343=VERTEX_POINT('',#7692);
#2344=VERTEX_POINT('',#7693);
#2345=VERTEX_POINT('',#7695);
#2346=VERTEX_POINT('',#7697);
#2347=VERTEX_POINT('',#7701);
#2348=VERTEX_POINT('',#7703);
#2349=VERTEX_POINT('',#7707);
#2350=VERTEX_POINT('',#7709);
#2351=VERTEX_POINT('',#7719);
#2352=VERTEX_POINT('',#7720);
#2353=VERTEX_POINT('',#7722);
#2354=VERTEX_POINT('',#7724);
#2355=VERTEX_POINT('',#7729);
#2356=VERTEX_POINT('',#7732);
#2357=VERTEX_POINT('',#7733);
#2358=VERTEX_POINT('',#7735);
#2359=VERTEX_POINT('',#7737);
#2360=VERTEX_POINT('',#7742);
#2361=VERTEX_POINT('',#7745);
#2362=VERTEX_POINT('',#7746);
#2363=VERTEX_POINT('',#7748);
#2364=VERTEX_POINT('',#7750);
#2365=VERTEX_POINT('',#7755);
#2366=VERTEX_POINT('',#7759);
#2367=VERTEX_POINT('',#7763);
#2368=VERTEX_POINT('',#7766);
#2369=VERTEX_POINT('',#7770);
#2370=VERTEX_POINT('',#7774);
#2371=VERTEX_POINT('',#7778);
#2372=VERTEX_POINT('',#7782);
#2373=VERTEX_POINT('',#7788);
#2374=VERTEX_POINT('',#7790);
#2375=VERTEX_POINT('',#7794);
#2376=VERTEX_POINT('',#7795);
#2377=VERTEX_POINT('',#7797);
#2378=VERTEX_POINT('',#7799);
#2379=VERTEX_POINT('',#7803);
#2380=VERTEX_POINT('',#7805);
#2381=VERTEX_POINT('',#7809);
#2382=VERTEX_POINT('',#7810);
#2383=VERTEX_POINT('',#7812);
#2384=VERTEX_POINT('',#7814);
#2385=VERTEX_POINT('',#7816);
#2386=VERTEX_POINT('',#7818);
#2387=VERTEX_POINT('',#7820);
#2388=VERTEX_POINT('',#7825);
#2389=VERTEX_POINT('',#7829);
#2390=VERTEX_POINT('',#7833);
#2391=VERTEX_POINT('',#7837);
#2392=VERTEX_POINT('',#7841);
#2393=VERTEX_POINT('',#7845);
#2394=VERTEX_POINT('',#7849);
#2395=VERTEX_POINT('',#7857);
#2396=VERTEX_POINT('',#7858);
#2397=VERTEX_POINT('',#7862);
#2398=VERTEX_POINT('',#7864);
#2399=VERTEX_POINT('',#7867);
#2400=VERTEX_POINT('',#7871);
#2401=VERTEX_POINT('',#7878);
#2402=VERTEX_POINT('',#7880);
#2403=VERTEX_POINT('',#7883);
#2404=VERTEX_POINT('',#7887);
#2405=VERTEX_POINT('',#7890);
#2406=VERTEX_POINT('',#7894);
#2407=VERTEX_POINT('',#7900);
#2408=VERTEX_POINT('',#7902);
#2409=VERTEX_POINT('',#7906);
#2410=VERTEX_POINT('',#7908);
#2411=VERTEX_POINT('',#8564);
#2412=VERTEX_POINT('',#8566);
#2413=VERTEX_POINT('',#8637);
#2414=VERTEX_POINT('',#8638);
#2415=VERTEX_POINT('',#8640);
#2416=VERTEX_POINT('',#8642);
#2417=VERTEX_POINT('',#8646);
#2418=VERTEX_POINT('',#8648);
#2419=VERTEX_POINT('',#8652);
#2420=VERTEX_POINT('',#8654);
#2421=VERTEX_POINT('',#8664);
#2422=VERTEX_POINT('',#8665);
#2423=VERTEX_POINT('',#8667);
#2424=VERTEX_POINT('',#8669);
#2425=VERTEX_POINT('',#8673);
#2426=VERTEX_POINT('',#8675);
#2427=VERTEX_POINT('',#8679);
#2428=VERTEX_POINT('',#8681);
#2429=VERTEX_POINT('',#8691);
#2430=VERTEX_POINT('',#8693);
#2431=VERTEX_POINT('',#8697);
#2432=VERTEX_POINT('',#8699);
#2433=VERTEX_POINT('',#8706);
#2434=VERTEX_POINT('',#8707);
#2435=VERTEX_POINT('',#8709);
#2436=VERTEX_POINT('',#8711);
#2437=VERTEX_POINT('',#8715);
#2438=VERTEX_POINT('',#8717);
#2439=VERTEX_POINT('',#8721);
#2440=VERTEX_POINT('',#8723);
#2441=VERTEX_POINT('',#8727);
#2442=VERTEX_POINT('',#8729);
#2443=VERTEX_POINT('',#8733);
#2444=VERTEX_POINT('',#8735);
#2445=VERTEX_POINT('',#8744);
#2446=VERTEX_POINT('',#8747);
#2447=VERTEX_POINT('',#8750);
#2448=VERTEX_POINT('',#8754);
#2449=VERTEX_POINT('',#8758);
#2450=VERTEX_POINT('',#8762);
#2451=VERTEX_POINT('',#8765);
#2452=VERTEX_POINT('',#8773);
#2453=VERTEX_POINT('',#8774);
#2454=VERTEX_POINT('',#8777);
#2455=VERTEX_POINT('',#8779);
#2456=VERTEX_POINT('',#8783);
#2457=VERTEX_POINT('',#8787);
#2458=VERTEX_POINT('',#8789);
#2459=VERTEX_POINT('',#8793);
#2460=VERTEX_POINT('',#8798);
#2461=VERTEX_POINT('',#8802);
#2462=VERTEX_POINT('',#8808);
#2463=VERTEX_POINT('',#8809);
#2464=VERTEX_POINT('',#8812);
#2465=VERTEX_POINT('',#8814);
#2466=VERTEX_POINT('',#8818);
#2467=VERTEX_POINT('',#8822);
#2468=VERTEX_POINT('',#8824);
#2469=VERTEX_POINT('',#8827);
#2470=VERTEX_POINT('',#8831);
#2471=VERTEX_POINT('',#8835);
#2472=VERTEX_POINT('',#8843);
#2473=VERTEX_POINT('',#8844);
#2474=VERTEX_POINT('',#8847);
#2475=VERTEX_POINT('',#8848);
#2476=VERTEX_POINT('',#8851);
#2477=VERTEX_POINT('',#8852);
#2478=VERTEX_POINT('',#8855);
#2479=VERTEX_POINT('',#8856);
#2480=VERTEX_POINT('',#8859);
#2481=VERTEX_POINT('',#8860);
#2482=VERTEX_POINT('',#8863);
#2483=VERTEX_POINT('',#8864);
#2484=VERTEX_POINT('',#8867);
#2485=VERTEX_POINT('',#8868);
#2486=VERTEX_POINT('',#8871);
#2487=VERTEX_POINT('',#8872);
#2488=VERTEX_POINT('',#8876);
#2489=VERTEX_POINT('',#8877);
#2490=VERTEX_POINT('',#8900);
#2491=VERTEX_POINT('',#8902);
#2492=VERTEX_POINT('',#8927);
#2493=VERTEX_POINT('',#8929);
#2494=VERTEX_POINT('',#8952);
#2495=VERTEX_POINT('',#8954);
#2496=VERTEX_POINT('',#8977);
#2497=VERTEX_POINT('',#8979);
#2498=VERTEX_POINT('',#8992);
#2499=VERTEX_POINT('',#8995);
#2500=VERTEX_POINT('',#9008);
#2501=VERTEX_POINT('',#9010);
#2502=VERTEX_POINT('',#9033);
#2503=VERTEX_POINT('',#9035);
#2504=VERTEX_POINT('',#9058);
#2505=VERTEX_POINT('',#9060);
#2506=VERTEX_POINT('',#9083);
#2507=VERTEX_POINT('',#9085);
#2508=VERTEX_POINT('',#9110);
#2509=VERTEX_POINT('',#9114);
#2510=VERTEX_POINT('',#9139);
#2511=VERTEX_POINT('',#9143);
#2512=VERTEX_POINT('',#9168);
#2513=VERTEX_POINT('',#9172);
#2514=VERTEX_POINT('',#9173);
#2515=VERTEX_POINT('',#9200);
#2516=VERTEX_POINT('',#9204);
#2517=VERTEX_POINT('',#9229);
#2518=VERTEX_POINT('',#9233);
#2519=VERTEX_POINT('',#9258);
#2520=VERTEX_POINT('',#9262);
#2521=VERTEX_POINT('',#9287);
#2522=VERTEX_POINT('',#9290);
#2523=VERTEX_POINT('',#9292);
#2524=VERTEX_POINT('',#9324);
#2525=VERTEX_POINT('',#9326);
#2526=VERTEX_POINT('',#9329);
#2527=VERTEX_POINT('',#9333);
#2528=VERTEX_POINT('',#9338);
#2529=VERTEX_POINT('',#9340);
#2530=VERTEX_POINT('',#9343);
#2531=VERTEX_POINT('',#9347);
#2532=VERTEX_POINT('',#9358);
#2533=VERTEX_POINT('',#9359);
#2534=VERTEX_POINT('',#9361);
#2535=VERTEX_POINT('',#9363);
#2536=VERTEX_POINT('',#9367);
#2537=VERTEX_POINT('',#9369);
#2538=VERTEX_POINT('',#9373);
#2539=VERTEX_POINT('',#9375);
#2540=VERTEX_POINT('',#9379);
#2541=VERTEX_POINT('',#9381);
#2542=VERTEX_POINT('',#9385);
#2543=VERTEX_POINT('',#9387);
#2544=VERTEX_POINT('',#9396);
#2545=VERTEX_POINT('',#9399);
#2546=VERTEX_POINT('',#9402);
#2547=VERTEX_POINT('',#9406);
#2548=VERTEX_POINT('',#9410);
#2549=VERTEX_POINT('',#9414);
#2550=VERTEX_POINT('',#9417);
#2551=VERTEX_POINT('',#9458);
#2552=VERTEX_POINT('',#9460);
#2553=VERTEX_POINT('',#9465);
#2554=VERTEX_POINT('',#9467);
#2555=VERTEX_POINT('',#9472);
#2556=VERTEX_POINT('',#9516);
#2557=VERTEX_POINT('',#9517);
#2558=VERTEX_POINT('',#9519);
#2559=VERTEX_POINT('',#9521);
#2560=VERTEX_POINT('',#9525);
#2561=VERTEX_POINT('',#9527);
#2562=VERTEX_POINT('',#9531);
#2563=VERTEX_POINT('',#9533);
#2564=VERTEX_POINT('',#9537);
#2565=VERTEX_POINT('',#9539);
#2566=VERTEX_POINT('',#9541);
#2567=VERTEX_POINT('',#9543);
#2568=VERTEX_POINT('',#9546);
#2569=VERTEX_POINT('',#9548);
#2570=VERTEX_POINT('',#9550);
#2571=VERTEX_POINT('',#9552);
#2572=VERTEX_POINT('',#9555);
#2573=VERTEX_POINT('',#9559);
#2574=VERTEX_POINT('',#9563);
#2575=VERTEX_POINT('',#9567);
#2576=VERTEX_POINT('',#9571);
#2577=VERTEX_POINT('',#9575);
#2578=VERTEX_POINT('',#9577);
#2579=VERTEX_POINT('',#9579);
#2580=VERTEX_POINT('',#9588);
#2581=VERTEX_POINT('',#9591);
#2582=VERTEX_POINT('',#9594);
#2583=VERTEX_POINT('',#9598);
#2584=VERTEX_POINT('',#9605);
#2585=VERTEX_POINT('',#9607);
#2586=VERTEX_POINT('',#9611);
#2587=VERTEX_POINT('',#9613);
#2588=VERTEX_POINT('',#9620);
#2589=VERTEX_POINT('',#9622);
#2590=VERTEX_POINT('',#9626);
#2591=VERTEX_POINT('',#9628);
#2592=VERTEX_POINT('',#9635);
#2593=VERTEX_POINT('',#9637);
#2594=VERTEX_POINT('',#9641);
#2595=VERTEX_POINT('',#9643);
#2596=VERTEX_POINT('',#9650);
#2597=VERTEX_POINT('',#9652);
#2598=VERTEX_POINT('',#9656);
#2599=VERTEX_POINT('',#9658);
#2600=VERTEX_POINT('',#9665);
#2601=VERTEX_POINT('',#9668);
#2602=VERTEX_POINT('',#9672);
#2603=VERTEX_POINT('',#9676);
#2604=VERTEX_POINT('',#9680);
#2605=VERTEX_POINT('',#9683);
#2606=VERTEX_POINT('',#9687);
#2607=VERTEX_POINT('',#9691);
#2608=VERTEX_POINT('',#9696);
#2609=VERTEX_POINT('',#9697);
#2610=VERTEX_POINT('',#9699);
#2611=VERTEX_POINT('',#9701);
#2612=VERTEX_POINT('',#9705);
#2613=VERTEX_POINT('',#9707);
#2614=VERTEX_POINT('',#9711);
#2615=VERTEX_POINT('',#9713);
#2616=VERTEX_POINT('',#9717);
#2617=VERTEX_POINT('',#9719);
#2618=VERTEX_POINT('',#9723);
#2619=VERTEX_POINT('',#9725);
#2620=EDGE_CURVE('',#2221,#2221,#1974,.T.);
#2621=EDGE_CURVE('',#2221,#2222,#1334,.T.);
#2622=EDGE_CURVE('',#2222,#2222,#1975,.T.);
#2623=EDGE_CURVE('',#2223,#2223,#1976,.T.);
#2624=EDGE_CURVE('',#2223,#2224,#1335,.T.);
#2625=EDGE_CURVE('',#2224,#2224,#1977,.T.);
#2626=EDGE_CURVE('',#2225,#2225,#1978,.T.);
#2627=EDGE_CURVE('',#2225,#2226,#1336,.T.);
#2628=EDGE_CURVE('',#2226,#2226,#1979,.T.);
#2629=EDGE_CURVE('',#2227,#2227,#1980,.T.);
#2630=EDGE_CURVE('',#2227,#2228,#1337,.T.);
#2631=EDGE_CURVE('',#2228,#2228,#1981,.T.);
#2632=EDGE_CURVE('',#2229,#2230,#1338,.T.);
#2633=EDGE_CURVE('',#2230,#2231,#1339,.T.);
#2634=EDGE_CURVE('',#2232,#2231,#1340,.T.);
#2635=EDGE_CURVE('',#2229,#2232,#1341,.T.);
#2636=EDGE_CURVE('',#2233,#2229,#1342,.T.);
#2637=EDGE_CURVE('',#2234,#2232,#1343,.T.);
#2638=EDGE_CURVE('',#2233,#2234,#1344,.T.);
#2639=EDGE_CURVE('',#2235,#2233,#1345,.T.);
#2640=EDGE_CURVE('',#2236,#2234,#1346,.T.);
#2641=EDGE_CURVE('',#2235,#2236,#1347,.T.);
#2642=EDGE_CURVE('',#2230,#2235,#1348,.T.);
#2643=EDGE_CURVE('',#2231,#2236,#1349,.T.);
#2644=EDGE_CURVE('',#2237,#2238,#1350,.T.);
#2645=EDGE_CURVE('',#2238,#2239,#1351,.T.);
#2646=EDGE_CURVE('',#2240,#2239,#1352,.T.);
#2647=EDGE_CURVE('',#2237,#2240,#1353,.T.);
#2648=EDGE_CURVE('',#2241,#2237,#1354,.T.);
#2649=EDGE_CURVE('',#2242,#2240,#1355,.T.);
#2650=EDGE_CURVE('',#2241,#2242,#1356,.T.);
#2651=EDGE_CURVE('',#2243,#2241,#1357,.T.);
#2652=EDGE_CURVE('',#2244,#2242,#1358,.T.);
#2653=EDGE_CURVE('',#2243,#2244,#1359,.T.);
#2654=EDGE_CURVE('',#2238,#2243,#1360,.T.);
#2655=EDGE_CURVE('',#2239,#2244,#1361,.T.);
#2656=EDGE_CURVE('',#2245,#2246,#1362,.T.);
#2657=EDGE_CURVE('',#2246,#2247,#1363,.T.);
#2658=EDGE_CURVE('',#2248,#2247,#1364,.T.);
#2659=EDGE_CURVE('',#2245,#2248,#1365,.T.);
#2660=EDGE_CURVE('',#2249,#2245,#1366,.T.);
#2661=EDGE_CURVE('',#2250,#2248,#1367,.T.);
#2662=EDGE_CURVE('',#2249,#2250,#1368,.T.);
#2663=EDGE_CURVE('',#2251,#2249,#1369,.T.);
#2664=EDGE_CURVE('',#2252,#2250,#1370,.T.);
#2665=EDGE_CURVE('',#2251,#2252,#1371,.T.);
#2666=EDGE_CURVE('',#2246,#2251,#1372,.T.);
#2667=EDGE_CURVE('',#2247,#2252,#1373,.T.);
#2668=EDGE_CURVE('',#2253,#2254,#1374,.T.);
#2669=EDGE_CURVE('',#2254,#2255,#1375,.T.);
#2670=EDGE_CURVE('',#2256,#2255,#1376,.T.);
#2671=EDGE_CURVE('',#2253,#2256,#1377,.T.);
#2672=EDGE_CURVE('',#2257,#2253,#1378,.T.);
#2673=EDGE_CURVE('',#2258,#2256,#1379,.T.);
#2674=EDGE_CURVE('',#2257,#2258,#1380,.T.);
#2675=EDGE_CURVE('',#2259,#2257,#1381,.T.);
#2676=EDGE_CURVE('',#2260,#2258,#1382,.T.);
#2677=EDGE_CURVE('',#2259,#2260,#1383,.T.);
#2678=EDGE_CURVE('',#2254,#2259,#1384,.T.);
#2679=EDGE_CURVE('',#2255,#2260,#1385,.T.);
#2680=EDGE_CURVE('',#2261,#2261,#1982,.T.);
#2681=EDGE_CURVE('',#2261,#2262,#1386,.T.);
#2682=EDGE_CURVE('',#2262,#2262,#1983,.T.);
#2683=EDGE_CURVE('',#2263,#2263,#1984,.T.);
#2684=EDGE_CURVE('',#2263,#2264,#1387,.T.);
#2685=EDGE_CURVE('',#2264,#2264,#1985,.T.);
#2686=EDGE_CURVE('',#2265,#2265,#1986,.T.);
#2687=EDGE_CURVE('',#2265,#2266,#1388,.T.);
#2688=EDGE_CURVE('',#2266,#2266,#1987,.T.);
#2689=EDGE_CURVE('',#2267,#2267,#1988,.T.);
#2690=EDGE_CURVE('',#2267,#2268,#1389,.T.);
#2691=EDGE_CURVE('',#2268,#2268,#1989,.T.);
#2692=EDGE_CURVE('',#2269,#2270,#1390,.T.);
#2693=EDGE_CURVE('',#2270,#2271,#1391,.T.);
#2694=EDGE_CURVE('',#2272,#2271,#1392,.T.);
#2695=EDGE_CURVE('',#2269,#2272,#1393,.T.);
#2696=EDGE_CURVE('',#2273,#2269,#1394,.T.);
#2697=EDGE_CURVE('',#2274,#2272,#1395,.T.);
#2698=EDGE_CURVE('',#2273,#2274,#1396,.T.);
#2699=EDGE_CURVE('',#2275,#2273,#1397,.T.);
#2700=EDGE_CURVE('',#2276,#2274,#1398,.T.);
#2701=EDGE_CURVE('',#2275,#2276,#1399,.T.);
#2702=EDGE_CURVE('',#2270,#2275,#1400,.T.);
#2703=EDGE_CURVE('',#2271,#2276,#1401,.T.);
#2704=EDGE_CURVE('',#2277,#2277,#1990,.T.);
#2705=EDGE_CURVE('',#2277,#2278,#1402,.T.);
#2706=EDGE_CURVE('',#2278,#2278,#1991,.T.);
#2707=EDGE_CURVE('',#2279,#2279,#1992,.T.);
#2708=EDGE_CURVE('',#2279,#2280,#1403,.T.);
#2709=EDGE_CURVE('',#2280,#2280,#1993,.T.);
#2710=EDGE_CURVE('',#2281,#2281,#1994,.T.);
#2711=EDGE_CURVE('',#2281,#2282,#1404,.T.);
#2712=EDGE_CURVE('',#2282,#2282,#1995,.T.);
#2713=EDGE_CURVE('',#2283,#2283,#1996,.T.);
#2714=EDGE_CURVE('',#2283,#2284,#1405,.T.);
#2715=EDGE_CURVE('',#2284,#2284,#1997,.T.);
#2716=EDGE_CURVE('',#2285,#2286,#1406,.T.);
#2717=EDGE_CURVE('',#2286,#2287,#1407,.T.);
#2718=EDGE_CURVE('',#2288,#2287,#1408,.T.);
#2719=EDGE_CURVE('',#2285,#2288,#1409,.T.);
#2720=EDGE_CURVE('',#2289,#2285,#1410,.T.);
#2721=EDGE_CURVE('',#2290,#2288,#1411,.T.);
#2722=EDGE_CURVE('',#2289,#2290,#1412,.T.);
#2723=EDGE_CURVE('',#2291,#2289,#1413,.T.);
#2724=EDGE_CURVE('',#2292,#2290,#1414,.T.);
#2725=EDGE_CURVE('',#2291,#2292,#1415,.T.);
#2726=EDGE_CURVE('',#2286,#2291,#1416,.T.);
#2727=EDGE_CURVE('',#2287,#2292,#1417,.T.);
#2728=EDGE_CURVE('',#2293,#2293,#1998,.T.);
#2729=EDGE_CURVE('',#2293,#2294,#1418,.T.);
#2730=EDGE_CURVE('',#2294,#2294,#1999,.T.);
#2731=EDGE_CURVE('',#2295,#2295,#2000,.T.);
#2732=EDGE_CURVE('',#2295,#2296,#1419,.T.);
#2733=EDGE_CURVE('',#2296,#2296,#2001,.T.);
#2734=EDGE_CURVE('',#2297,#2297,#2002,.T.);
#2735=EDGE_CURVE('',#2297,#2298,#1420,.T.);
#2736=EDGE_CURVE('',#2298,#2298,#2003,.T.);
#2737=EDGE_CURVE('',#2299,#2299,#2004,.T.);
#2738=EDGE_CURVE('',#2299,#2300,#1421,.T.);
#2739=EDGE_CURVE('',#2300,#2300,#2005,.T.);
#2740=EDGE_CURVE('',#2301,#2301,#2006,.T.);
#2741=EDGE_CURVE('',#2302,#2302,#2007,.T.);
#2742=EDGE_CURVE('',#2302,#2301,#1422,.T.);
#2743=EDGE_CURVE('',#2303,#2304,#1423,.T.);
#2744=EDGE_CURVE('',#2304,#2305,#1424,.T.);
#2745=EDGE_CURVE('',#2305,#2306,#1425,.T.);
#2746=EDGE_CURVE('',#2306,#2303,#2008,.T.);
#2747=EDGE_CURVE('',#2307,#2303,#1426,.T.);
#2748=EDGE_CURVE('',#2307,#2308,#1427,.T.);
#2749=EDGE_CURVE('',#2308,#2304,#1428,.T.);
#2750=EDGE_CURVE('',#2306,#2309,#1429,.T.);
#2751=EDGE_CURVE('',#2310,#2305,#1430,.T.);
#2752=EDGE_CURVE('',#2310,#2309,#1431,.T.);
#2753=EDGE_CURVE('',#2308,#2310,#1432,.T.);
#2754=EDGE_CURVE('',#2309,#2307,#2009,.T.);
#2755=EDGE_CURVE('',#2311,#2312,#2010,.T.);
#2756=EDGE_CURVE('',#2311,#2312,#2011,.T.);
#2757=EDGE_CURVE('',#2313,#2313,#2012,.T.);
#2758=EDGE_CURVE('',#2314,#2311,#1433,.T.);
#2759=EDGE_CURVE('',#2315,#2314,#2013,.T.);
#2760=EDGE_CURVE('',#2312,#2315,#1434,.T.);
#2761=EDGE_CURVE('',#2316,#2317,#2014,.T.);
#2762=EDGE_CURVE('',#2316,#2317,#2015,.T.);
#2763=EDGE_CURVE('',#2318,#2318,#2016,.T.);
#2764=EDGE_CURVE('',#2319,#2316,#1435,.T.);
#2765=EDGE_CURVE('',#2320,#2319,#2017,.T.);
#2766=EDGE_CURVE('',#2317,#2320,#1436,.T.);
#2767=EDGE_CURVE('',#2321,#2322,#2018,.T.);
#2768=EDGE_CURVE('',#2321,#2322,#2019,.T.);
#2769=EDGE_CURVE('',#2323,#2323,#2020,.T.);
#2770=EDGE_CURVE('',#2324,#2321,#1437,.T.);
#2771=EDGE_CURVE('',#2325,#2324,#2021,.T.);
#2772=EDGE_CURVE('',#2322,#2325,#1438,.T.);
#2773=EDGE_CURVE('',#2324,#2315,#2022,.T.);
#2774=EDGE_CURVE('',#2326,#2325,#2023,.T.);
#2775=EDGE_CURVE('',#2326,#2327,#1439,.T.);
#2776=EDGE_CURVE('',#2327,#2327,#2024,.T.);
#2777=EDGE_CURVE('',#2319,#2326,#2025,.T.);
#2778=EDGE_CURVE('',#2314,#2320,#2026,.T.);
#2779=EDGE_CURVE('',#2328,#2328,#2027,.T.);
#2780=EDGE_CURVE('',#2328,#2313,#1440,.T.);
#2781=EDGE_CURVE('',#2329,#2329,#2028,.T.);
#2782=EDGE_CURVE('',#2329,#2318,#1441,.T.);
#2783=EDGE_CURVE('',#2330,#2330,#2029,.T.);
#2784=EDGE_CURVE('',#2330,#2323,#1442,.T.);
#2785=EDGE_CURVE('',#2331,#2331,#2030,.T.);
#2786=EDGE_CURVE('',#2331,#2332,#1443,.T.);
#2787=EDGE_CURVE('',#2332,#2332,#2031,.T.);
#2788=EDGE_CURVE('',#2333,#2333,#2032,.T.);
#2789=EDGE_CURVE('',#2333,#2334,#1444,.T.);
#2790=EDGE_CURVE('',#2334,#2334,#2033,.T.);
#2791=EDGE_CURVE('',#2335,#2335,#2034,.T.);
#2792=EDGE_CURVE('',#2335,#2336,#1445,.T.);
#2793=EDGE_CURVE('',#2336,#2336,#2035,.T.);
#2794=EDGE_CURVE('',#2337,#2337,#2036,.T.);
#2795=EDGE_CURVE('',#2337,#2338,#1446,.T.);
#2796=EDGE_CURVE('',#2338,#2338,#2037,.T.);
#2797=EDGE_CURVE('',#2339,#2339,#2038,.T.);
#2798=EDGE_CURVE('',#2339,#2340,#1447,.T.);
#2799=EDGE_CURVE('',#2340,#2340,#2039,.T.);
#2800=EDGE_CURVE('',#2341,#2341,#2040,.T.);
#2801=EDGE_CURVE('',#2341,#2342,#1448,.T.);
#2802=EDGE_CURVE('',#2342,#2342,#2041,.T.);
#2803=EDGE_CURVE('',#2343,#2344,#1449,.T.);
#2804=EDGE_CURVE('',#2344,#2345,#1450,.T.);
#2805=EDGE_CURVE('',#2345,#2346,#1451,.T.);
#2806=EDGE_CURVE('',#2346,#2343,#2042,.T.);
#2807=EDGE_CURVE('',#2347,#2343,#1452,.T.);
#2808=EDGE_CURVE('',#2347,#2348,#1453,.T.);
#2809=EDGE_CURVE('',#2348,#2344,#1454,.T.);
#2810=EDGE_CURVE('',#2346,#2349,#1455,.T.);
#2811=EDGE_CURVE('',#2350,#2345,#1456,.T.);
#2812=EDGE_CURVE('',#2350,#2349,#1457,.T.);
#2813=EDGE_CURVE('',#2348,#2350,#1458,.T.);
#2814=EDGE_CURVE('',#2349,#2347,#2043,.T.);
#2815=EDGE_CURVE('',#2351,#2352,#1459,.T.);
#2816=EDGE_CURVE('',#2351,#2353,#2044,.T.);
#2817=EDGE_CURVE('',#2354,#2353,#1460,.T.);
#2818=EDGE_CURVE('',#2352,#2354,#2045,.T.);
#2819=EDGE_CURVE('',#2353,#2351,#2046,.T.);
#2820=EDGE_CURVE('',#2355,#2355,#2047,.T.);
#2821=EDGE_CURVE('',#2356,#2357,#1461,.T.);
#2822=EDGE_CURVE('',#2356,#2358,#2048,.T.);
#2823=EDGE_CURVE('',#2359,#2358,#1462,.T.);
#2824=EDGE_CURVE('',#2357,#2359,#2049,.T.);
#2825=EDGE_CURVE('',#2358,#2356,#2050,.T.);
#2826=EDGE_CURVE('',#2360,#2360,#2051,.T.);
#2827=EDGE_CURVE('',#2361,#2362,#1463,.T.);
#2828=EDGE_CURVE('',#2361,#2363,#2052,.T.);
#2829=EDGE_CURVE('',#2364,#2363,#1464,.T.);
#2830=EDGE_CURVE('',#2362,#2364,#2053,.T.);
#2831=EDGE_CURVE('',#2363,#2361,#2054,.T.);
#2832=EDGE_CURVE('',#2365,#2365,#2055,.T.);
#2833=EDGE_CURVE('',#2362,#2354,#2056,.T.);
#2834=EDGE_CURVE('',#2366,#2364,#2057,.T.);
#2835=EDGE_CURVE('',#2357,#2366,#2058,.T.);
#2836=EDGE_CURVE('',#2352,#2359,#2059,.T.);
#2837=EDGE_CURVE('',#2367,#2367,#2060,.T.);
#2838=EDGE_CURVE('',#2355,#2368,#1465,.T.);
#2839=EDGE_CURVE('',#2368,#2368,#2061,.T.);
#2840=EDGE_CURVE('',#2360,#2369,#1466,.T.);
#2841=EDGE_CURVE('',#2369,#2369,#2062,.T.);
#2842=EDGE_CURVE('',#2365,#2370,#1467,.T.);
#2843=EDGE_CURVE('',#2370,#2370,#2063,.T.);
#2844=EDGE_CURVE('',#2371,#2371,#2064,.T.);
#2845=EDGE_CURVE('',#2371,#2367,#1468,.T.);
#2846=EDGE_CURVE('',#2372,#2372,#2065,.T.);
#2847=EDGE_CURVE('',#2372,#2366,#1469,.T.);
#2848=EDGE_CURVE('',#2373,#2373,#2066,.T.);
#2849=EDGE_CURVE('',#2373,#2374,#1470,.T.);
#2850=EDGE_CURVE('',#2374,#2374,#2067,.T.);
#2851=EDGE_CURVE('',#2375,#2376,#1471,.T.);
#2852=EDGE_CURVE('',#2375,#2377,#1472,.T.);
#2853=EDGE_CURVE('',#2378,#2377,#1473,.T.);
#2854=EDGE_CURVE('',#2376,#2378,#1474,.T.);
#2855=EDGE_CURVE('',#2379,#2378,#1475,.T.);
#2856=EDGE_CURVE('',#2377,#2380,#1476,.T.);
#2857=EDGE_CURVE('',#2380,#2379,#1477,.T.);
#2858=EDGE_CURVE('',#2381,#2382,#1478,.T.);
#2859=EDGE_CURVE('',#2381,#2383,#1479,.T.);
#2860=EDGE_CURVE('',#2383,#2384,#1480,.T.);
#2861=EDGE_CURVE('',#2384,#2385,#1481,.T.);
#2862=EDGE_CURVE('',#2385,#2386,#1482,.T.);
#2863=EDGE_CURVE('',#2386,#2387,#1483,.T.);
#2864=EDGE_CURVE('',#2376,#2387,#1484,.T.);
#2865=EDGE_CURVE('',#2382,#2379,#1485,.T.);
#2866=EDGE_CURVE('',#2382,#2388,#1486,.T.);
#2867=EDGE_CURVE('',#2388,#2380,#1487,.T.);
#2868=EDGE_CURVE('',#2389,#2387,#1488,.T.);
#2869=EDGE_CURVE('',#2389,#2375,#1489,.T.);
#2870=EDGE_CURVE('',#2388,#2390,#1490,.T.);
#2871=EDGE_CURVE('',#2381,#2390,#1491,.T.);
#2872=EDGE_CURVE('',#2390,#2391,#1492,.T.);
#2873=EDGE_CURVE('',#2391,#2383,#1493,.T.);
#2874=EDGE_CURVE('',#2392,#2386,#1494,.T.);
#2875=EDGE_CURVE('',#2392,#2389,#1495,.T.);
#2876=EDGE_CURVE('',#2393,#2392,#1496,.T.);
#2877=EDGE_CURVE('',#2393,#2385,#1497,.T.);
#2878=EDGE_CURVE('',#2394,#2393,#1498,.T.);
#2879=EDGE_CURVE('',#2394,#2384,#1499,.T.);
#2880=EDGE_CURVE('',#2391,#2394,#1500,.T.);
#2881=EDGE_CURVE('',#2395,#2396,#2068,.T.);
#2882=EDGE_CURVE('',#2397,#2397,#2069,.T.);
#2883=EDGE_CURVE('',#2398,#2398,#2070,.T.);
#2884=EDGE_CURVE('',#2399,#2399,#2071,.T.);
#2885=EDGE_CURVE('',#2399,#2397,#1501,.T.);
#2886=EDGE_CURVE('',#2398,#2400,#1502,.T.);
#2887=EDGE_CURVE('',#2400,#2400,#2072,.T.);
#2888=EDGE_CURVE('',#2401,#2401,#2073,.T.);
#2889=EDGE_CURVE('',#2402,#2402,#2074,.T.);
#2890=EDGE_CURVE('',#2401,#2403,#1503,.T.);
#2891=EDGE_CURVE('',#2403,#2403,#2075,.T.);
#2892=EDGE_CURVE('',#2404,#2404,#2076,.T.);
#2893=EDGE_CURVE('',#2405,#2405,#2077,.T.);
#2894=EDGE_CURVE('',#2405,#2404,#1504,.T.);
#2895=EDGE_CURVE('',#2406,#2406,#2078,.T.);
#2896=EDGE_CURVE('',#2406,#2402,#1505,.T.);
#2897=EDGE_CURVE('',#2407,#2407,#2079,.T.);
#2898=EDGE_CURVE('',#2407,#2408,#1506,.T.);
#2899=EDGE_CURVE('',#2408,#2408,#2080,.T.);
#2900=EDGE_CURVE('',#2409,#2409,#2081,.T.);
#2901=EDGE_CURVE('',#2409,#2410,#1507,.T.);
#2902=EDGE_CURVE('',#2410,#2410,#2082,.T.);
#2903=EDGE_CURVE('',#2411,#2411,#2083,.T.);
#2904=EDGE_CURVE('',#2411,#2412,#221,.T.);
#2905=EDGE_CURVE('',#2412,#2412,#2084,.T.);
#2906=EDGE_CURVE('',#2413,#2414,#1508,.T.);
#2907=EDGE_CURVE('',#2414,#2415,#1509,.T.);
#2908=EDGE_CURVE('',#2416,#2415,#1510,.T.);
#2909=EDGE_CURVE('',#2413,#2416,#1511,.T.);
#2910=EDGE_CURVE('',#2417,#2413,#1512,.T.);
#2911=EDGE_CURVE('',#2418,#2416,#1513,.T.);
#2912=EDGE_CURVE('',#2417,#2418,#1514,.T.);
#2913=EDGE_CURVE('',#2419,#2417,#1515,.T.);
#2914=EDGE_CURVE('',#2420,#2418,#1516,.T.);
#2915=EDGE_CURVE('',#2419,#2420,#1517,.T.);
#2916=EDGE_CURVE('',#2414,#2419,#1518,.T.);
#2917=EDGE_CURVE('',#2415,#2420,#1519,.T.);
#2918=EDGE_CURVE('',#2421,#2422,#1520,.T.);
#2919=EDGE_CURVE('',#2422,#2423,#1521,.T.);
#2920=EDGE_CURVE('',#2424,#2423,#1522,.T.);
#2921=EDGE_CURVE('',#2421,#2424,#1523,.T.);
#2922=EDGE_CURVE('',#2425,#2421,#1524,.T.);
#2923=EDGE_CURVE('',#2426,#2424,#1525,.T.);
#2924=EDGE_CURVE('',#2425,#2426,#1526,.T.);
#2925=EDGE_CURVE('',#2427,#2425,#1527,.T.);
#2926=EDGE_CURVE('',#2428,#2426,#1528,.T.);
#2927=EDGE_CURVE('',#2427,#2428,#1529,.T.);
#2928=EDGE_CURVE('',#2422,#2427,#1530,.T.);
#2929=EDGE_CURVE('',#2423,#2428,#1531,.T.);
#2930=EDGE_CURVE('',#2429,#2429,#2085,.T.);
#2931=EDGE_CURVE('',#2429,#2430,#1532,.T.);
#2932=EDGE_CURVE('',#2430,#2430,#2086,.T.);
#2933=EDGE_CURVE('',#2431,#2431,#2087,.T.);
#2934=EDGE_CURVE('',#2431,#2432,#1533,.T.);
#2935=EDGE_CURVE('',#2432,#2432,#2088,.T.);
#2936=EDGE_CURVE('',#2433,#2434,#1534,.T.);
#2937=EDGE_CURVE('',#2434,#2435,#1535,.T.);
#2938=EDGE_CURVE('',#2435,#2436,#1536,.T.);
#2939=EDGE_CURVE('',#2433,#2436,#1537,.T.);
#2940=EDGE_CURVE('',#2434,#2437,#1538,.T.);
#2941=EDGE_CURVE('',#2437,#2438,#1539,.T.);
#2942=EDGE_CURVE('',#2438,#2435,#1540,.T.);
#2943=EDGE_CURVE('',#2437,#2439,#1541,.T.);
#2944=EDGE_CURVE('',#2439,#2440,#1542,.T.);
#2945=EDGE_CURVE('',#2440,#2438,#1543,.T.);
#2946=EDGE_CURVE('',#2439,#2441,#1544,.T.);
#2947=EDGE_CURVE('',#2441,#2442,#1545,.T.);
#2948=EDGE_CURVE('',#2442,#2440,#1546,.T.);
#2949=EDGE_CURVE('',#2441,#2443,#1547,.T.);
#2950=EDGE_CURVE('',#2443,#2444,#1548,.T.);
#2951=EDGE_CURVE('',#2444,#2442,#1549,.T.);
#2952=EDGE_CURVE('',#2443,#2433,#1550,.T.);
#2953=EDGE_CURVE('',#2436,#2444,#1551,.T.);
#2954=EDGE_CURVE('',#2445,#2445,#2089,.T.);
#2955=EDGE_CURVE('',#2446,#2446,#2090,.T.);
#2956=EDGE_CURVE('',#2447,#2447,#2091,.T.);
#2957=EDGE_CURVE('',#2447,#2446,#1552,.T.);
#2958=EDGE_CURVE('',#2448,#2448,#2092,.T.);
#2959=EDGE_CURVE('',#2448,#2447,#1553,.T.);
#2960=EDGE_CURVE('',#2449,#2449,#2093,.T.);
#2961=EDGE_CURVE('',#2449,#2448,#1554,.T.);
#2962=EDGE_CURVE('',#2450,#2450,#2094,.T.);
#2963=EDGE_CURVE('',#2451,#2451,#2095,.F.);
#2964=EDGE_CURVE('',#2451,#2450,#1555,.T.);
#2965=EDGE_CURVE('',#2445,#2451,#1556,.T.);
#2966=EDGE_CURVE('',#2452,#2453,#2096,.T.);
#2967=EDGE_CURVE('',#2453,#2452,#2097,.T.);
#2968=EDGE_CURVE('',#2453,#2454,#2098,.T.);
#2969=EDGE_CURVE('',#2455,#2454,#2099,.T.);
#2970=EDGE_CURVE('',#2454,#2455,#2100,.T.);
#2971=EDGE_CURVE('',#2455,#2456,#1557,.T.);
#2972=EDGE_CURVE('',#2456,#2456,#2101,.T.);
#2973=EDGE_CURVE('',#2457,#2457,#2102,.T.);
#2974=EDGE_CURVE('',#2457,#2458,#1558,.T.);
#2975=EDGE_CURVE('',#2458,#2458,#2103,.T.);
#2976=EDGE_CURVE('',#2458,#2459,#1559,.T.);
#2977=EDGE_CURVE('',#2459,#2459,#2104,.T.);
#2978=EDGE_CURVE('',#2460,#2460,#2105,.T.);
#2979=EDGE_CURVE('',#2460,#2452,#1560,.T.);
#2980=EDGE_CURVE('',#2461,#2461,#2106,.T.);
#2981=EDGE_CURVE('',#2461,#2457,#1561,.T.);
#2982=EDGE_CURVE('',#2462,#2463,#2107,.T.);
#2983=EDGE_CURVE('',#2463,#2462,#2108,.T.);
#2984=EDGE_CURVE('',#2463,#2464,#2109,.T.);
#2985=EDGE_CURVE('',#2465,#2464,#2110,.T.);
#2986=EDGE_CURVE('',#2464,#2465,#2111,.T.);
#2987=EDGE_CURVE('',#2466,#2466,#2112,.T.);
#2988=EDGE_CURVE('',#2466,#2465,#1562,.T.);
#2989=EDGE_CURVE('',#2467,#2467,#2113,.T.);
#2990=EDGE_CURVE('',#2468,#2468,#2114,.T.);
#2991=EDGE_CURVE('',#2469,#2469,#2115,.T.);
#2992=EDGE_CURVE('',#2469,#2467,#1563,.T.);
#2993=EDGE_CURVE('',#2470,#2470,#2116,.T.);
#2994=EDGE_CURVE('',#2470,#2469,#1564,.T.);
#2995=EDGE_CURVE('',#2471,#2471,#2117,.T.);
#2996=EDGE_CURVE('',#2471,#2470,#1565,.T.);
#2997=EDGE_CURVE('',#2462,#2468,#1566,.T.);
#2998=EDGE_CURVE('',#2472,#2473,#2118,.T.);
#2999=EDGE_CURVE('',#2474,#2475,#2119,.T.);
#3000=EDGE_CURVE('',#2476,#2477,#2120,.T.);
#3001=EDGE_CURVE('',#2478,#2479,#2121,.T.);
#3002=EDGE_CURVE('',#2480,#2481,#2122,.T.);
#3003=EDGE_CURVE('',#2482,#2483,#2123,.T.);
#3004=EDGE_CURVE('',#2484,#2485,#2124,.T.);
#3005=EDGE_CURVE('',#2486,#2487,#2125,.T.);
#3006=EDGE_CURVE('',#2488,#2489,#222,.T.);
#3007=EDGE_CURVE('',#2490,#2488,#2126,.T.);
#3008=EDGE_CURVE('',#2491,#2490,#223,.T.);
#3009=EDGE_CURVE('',#2489,#2491,#2127,.T.);
#3010=EDGE_CURVE('',#2492,#2490,#2128,.T.);
#3011=EDGE_CURVE('',#2492,#2493,#224,.T.);
#3012=EDGE_CURVE('',#2494,#2493,#2129,.T.);
#3013=EDGE_CURVE('',#2494,#2495,#225,.T.);
#3014=EDGE_CURVE('',#2496,#2495,#2130,.T.);
#3015=EDGE_CURVE('',#2496,#2497,#226,.T.);
#3016=EDGE_CURVE('',#2497,#2498,#1567,.T.);
#3017=EDGE_CURVE('',#2498,#2498,#2131,.T.);
#3018=EDGE_CURVE('',#2497,#2499,#227,.T.);
#3019=EDGE_CURVE('',#2500,#2499,#2132,.T.);
#3020=EDGE_CURVE('',#2500,#2501,#228,.T.);
#3021=EDGE_CURVE('',#2502,#2501,#2133,.T.);
#3022=EDGE_CURVE('',#2502,#2503,#229,.T.);
#3023=EDGE_CURVE('',#2504,#2503,#2134,.T.);
#3024=EDGE_CURVE('',#2504,#2505,#230,.T.);
#3025=EDGE_CURVE('',#2506,#2505,#2135,.T.);
#3026=EDGE_CURVE('',#2506,#2507,#231,.T.);
#3027=EDGE_CURVE('',#2491,#2507,#2136,.T.);
#3028=EDGE_CURVE('',#2488,#2508,#2137,.T.);
#3029=EDGE_CURVE('',#2508,#2492,#2138,.T.);
#3030=EDGE_CURVE('',#2509,#2508,#232,.T.);
#3031=EDGE_CURVE('',#2493,#2509,#2139,.T.);
#3032=EDGE_CURVE('',#2509,#2510,#2140,.T.);
#3033=EDGE_CURVE('',#2510,#2494,#2141,.T.);
#3034=EDGE_CURVE('',#2511,#2510,#233,.T.);
#3035=EDGE_CURVE('',#2495,#2511,#2142,.T.);
#3036=EDGE_CURVE('',#2511,#2512,#2143,.T.);
#3037=EDGE_CURVE('',#2512,#2496,#2144,.T.);
#3038=EDGE_CURVE('',#2513,#2514,#234,.T.);
#3039=EDGE_CURVE('',#2499,#2513,#2145,.T.);
#3040=EDGE_CURVE('',#2514,#2512,#235,.T.);
#3041=EDGE_CURVE('',#2513,#2515,#2146,.T.);
#3042=EDGE_CURVE('',#2515,#2500,#2147,.T.);
#3043=EDGE_CURVE('',#2516,#2515,#236,.T.);
#3044=EDGE_CURVE('',#2501,#2516,#2148,.T.);
#3045=EDGE_CURVE('',#2516,#2517,#2149,.T.);
#3046=EDGE_CURVE('',#2517,#2502,#2150,.T.);
#3047=EDGE_CURVE('',#2518,#2517,#237,.T.);
#3048=EDGE_CURVE('',#2503,#2518,#2151,.T.);
#3049=EDGE_CURVE('',#2518,#2519,#2152,.T.);
#3050=EDGE_CURVE('',#2519,#2504,#2153,.T.);
#3051=EDGE_CURVE('',#2520,#2519,#238,.T.);
#3052=EDGE_CURVE('',#2505,#2520,#2154,.T.);
#3053=EDGE_CURVE('',#2521,#2521,#2155,.T.);
#3054=EDGE_CURVE('',#2521,#2514,#1568,.T.);
#3055=EDGE_CURVE('',#2522,#2489,#2156,.T.);
#3056=EDGE_CURVE('',#2522,#2523,#239,.T.);
#3057=EDGE_CURVE('',#2520,#2523,#2157,.T.);
#3058=EDGE_CURVE('',#2507,#2522,#2158,.T.);
#3059=EDGE_CURVE('',#2523,#2506,#2159,.T.);
#3060=EDGE_CURVE('',#2524,#2524,#2160,.T.);
#3061=EDGE_CURVE('',#2525,#2525,#2161,.T.);
#3062=EDGE_CURVE('',#2526,#2526,#2162,.T.);
#3063=EDGE_CURVE('',#2526,#2524,#1569,.T.);
#3064=EDGE_CURVE('',#2527,#2527,#2163,.T.);
#3065=EDGE_CURVE('',#2527,#2525,#1570,.T.);
#3066=EDGE_CURVE('',#2528,#2528,#2164,.T.);
#3067=EDGE_CURVE('',#2529,#2529,#2165,.T.);
#3068=EDGE_CURVE('',#2530,#2530,#2166,.T.);
#3069=EDGE_CURVE('',#2530,#2528,#1571,.T.);
#3070=EDGE_CURVE('',#2531,#2531,#2167,.T.);
#3071=EDGE_CURVE('',#2531,#2529,#1572,.T.);
#3072=EDGE_CURVE('',#2532,#2533,#1573,.T.);
#3073=EDGE_CURVE('',#2533,#2534,#1574,.T.);
#3074=EDGE_CURVE('',#2534,#2535,#1575,.T.);
#3075=EDGE_CURVE('',#2532,#2535,#1576,.T.);
#3076=EDGE_CURVE('',#2533,#2536,#1577,.T.);
#3077=EDGE_CURVE('',#2536,#2537,#1578,.T.);
#3078=EDGE_CURVE('',#2537,#2534,#1579,.T.);
#3079=EDGE_CURVE('',#2536,#2538,#1580,.T.);
#3080=EDGE_CURVE('',#2538,#2539,#1581,.T.);
#3081=EDGE_CURVE('',#2539,#2537,#1582,.T.);
#3082=EDGE_CURVE('',#2538,#2540,#1583,.T.);
#3083=EDGE_CURVE('',#2540,#2541,#1584,.T.);
#3084=EDGE_CURVE('',#2541,#2539,#1585,.T.);
#3085=EDGE_CURVE('',#2540,#2542,#1586,.T.);
#3086=EDGE_CURVE('',#2542,#2543,#1587,.T.);
#3087=EDGE_CURVE('',#2543,#2541,#1588,.T.);
#3088=EDGE_CURVE('',#2542,#2532,#1589,.T.);
#3089=EDGE_CURVE('',#2535,#2543,#1590,.T.);
#3090=EDGE_CURVE('',#2544,#2544,#2168,.T.);
#3091=EDGE_CURVE('',#2545,#2545,#2169,.T.);
#3092=EDGE_CURVE('',#2546,#2546,#2170,.T.);
#3093=EDGE_CURVE('',#2546,#2545,#1591,.T.);
#3094=EDGE_CURVE('',#2547,#2547,#2171,.T.);
#3095=EDGE_CURVE('',#2547,#2546,#1592,.T.);
#3096=EDGE_CURVE('',#2548,#2548,#2172,.T.);
#3097=EDGE_CURVE('',#2548,#2547,#1593,.T.);
#3098=EDGE_CURVE('',#2549,#2549,#2173,.T.);
#3099=EDGE_CURVE('',#2550,#2550,#2174,.F.);
#3100=EDGE_CURVE('',#2550,#2549,#1594,.T.);
#3101=EDGE_CURVE('',#2544,#2550,#1595,.T.);
#3102=EDGE_CURVE('',#2551,#2551,#2175,.T.);
#3103=EDGE_CURVE('',#2551,#2552,#1596,.T.);
#3104=EDGE_CURVE('',#2552,#2552,#2176,.T.);
#3105=EDGE_CURVE('',#2553,#2553,#2177,.T.);
#3106=EDGE_CURVE('',#2553,#2554,#1597,.T.);
#3107=EDGE_CURVE('',#2554,#2554,#2178,.T.);
#3108=EDGE_CURVE('',#2555,#2555,#240,.T.);
#3109=EDGE_CURVE('',#2556,#2557,#1598,.T.);
#3110=EDGE_CURVE('',#2558,#2556,#2179,.T.);
#3111=EDGE_CURVE('',#2559,#2558,#1599,.T.);
#3112=EDGE_CURVE('',#2559,#2557,#2180,.T.);
#3113=EDGE_CURVE('',#2557,#2560,#1600,.T.);
#3114=EDGE_CURVE('',#2561,#2559,#1601,.T.);
#3115=EDGE_CURVE('',#2561,#2560,#2181,.T.);
#3116=EDGE_CURVE('',#2560,#2562,#1602,.T.);
#3117=EDGE_CURVE('',#2563,#2561,#1603,.T.);
#3118=EDGE_CURVE('',#2562,#2563,#2182,.T.);
#3119=EDGE_CURVE('',#2564,#2562,#1604,.T.);
#3120=EDGE_CURVE('',#2564,#2565,#1605,.T.);
#3121=EDGE_CURVE('',#2565,#2566,#1606,.T.);
#3122=EDGE_CURVE('',#2567,#2566,#1607,.T.);
#3123=EDGE_CURVE('',#2556,#2567,#1608,.T.);
#3124=EDGE_CURVE('',#2568,#2568,#2183,.T.);
#3125=EDGE_CURVE('',#2569,#2569,#2184,.T.);
#3126=EDGE_CURVE('',#2570,#2570,#2185,.T.);
#3127=EDGE_CURVE('',#2571,#2571,#2186,.T.);
#3128=EDGE_CURVE('',#2563,#2572,#1609,.T.);
#3129=EDGE_CURVE('',#2572,#2564,#2187,.T.);
#3130=EDGE_CURVE('',#2571,#2573,#1610,.T.);
#3131=EDGE_CURVE('',#2573,#2573,#2188,.T.);
#3132=EDGE_CURVE('',#2570,#2574,#1611,.T.);
#3133=EDGE_CURVE('',#2574,#2574,#2189,.T.);
#3134=EDGE_CURVE('',#2569,#2575,#1612,.T.);
#3135=EDGE_CURVE('',#2575,#2575,#2190,.T.);
#3136=EDGE_CURVE('',#2568,#2576,#1613,.T.);
#3137=EDGE_CURVE('',#2576,#2576,#2191,.T.);
#3138=EDGE_CURVE('',#2577,#2558,#1614,.T.);
#3139=EDGE_CURVE('',#2578,#2577,#1615,.T.);
#3140=EDGE_CURVE('',#2579,#2578,#1616,.T.);
#3141=EDGE_CURVE('',#2579,#2572,#1617,.T.);
#3142=EDGE_CURVE('',#2565,#2579,#1618,.T.);
#3143=EDGE_CURVE('',#2566,#2578,#1619,.T.);
#3144=EDGE_CURVE('',#2577,#2567,#2192,.T.);
#3145=EDGE_CURVE('',#2580,#2580,#2193,.T.);
#3146=EDGE_CURVE('',#2581,#2581,#2194,.T.);
#3147=EDGE_CURVE('',#2580,#2582,#1620,.T.);
#3148=EDGE_CURVE('',#2582,#2582,#2195,.T.);
#3149=EDGE_CURVE('',#2583,#2583,#2196,.T.);
#3150=EDGE_CURVE('',#2583,#2581,#1621,.T.);
#3151=EDGE_CURVE('',#2584,#2584,#2197,.T.);
#3152=EDGE_CURVE('',#2584,#2585,#1622,.T.);
#3153=EDGE_CURVE('',#2585,#2585,#2198,.T.);
#3154=EDGE_CURVE('',#2586,#2586,#2199,.T.);
#3155=EDGE_CURVE('',#2586,#2587,#1623,.T.);
#3156=EDGE_CURVE('',#2587,#2587,#2200,.T.);
#3157=EDGE_CURVE('',#2588,#2588,#2201,.T.);
#3158=EDGE_CURVE('',#2588,#2589,#1624,.T.);
#3159=EDGE_CURVE('',#2589,#2589,#2202,.T.);
#3160=EDGE_CURVE('',#2590,#2590,#2203,.T.);
#3161=EDGE_CURVE('',#2590,#2591,#1625,.T.);
#3162=EDGE_CURVE('',#2591,#2591,#2204,.T.);
#3163=EDGE_CURVE('',#2592,#2592,#2205,.T.);
#3164=EDGE_CURVE('',#2592,#2593,#1626,.T.);
#3165=EDGE_CURVE('',#2593,#2593,#2206,.T.);
#3166=EDGE_CURVE('',#2594,#2594,#2207,.T.);
#3167=EDGE_CURVE('',#2594,#2595,#1627,.T.);
#3168=EDGE_CURVE('',#2595,#2595,#2208,.T.);
#3169=EDGE_CURVE('',#2596,#2596,#2209,.T.);
#3170=EDGE_CURVE('',#2596,#2597,#1628,.T.);
#3171=EDGE_CURVE('',#2597,#2597,#2210,.T.);
#3172=EDGE_CURVE('',#2598,#2598,#2211,.T.);
#3173=EDGE_CURVE('',#2598,#2599,#1629,.T.);
#3174=EDGE_CURVE('',#2599,#2599,#2212,.T.);
#3175=EDGE_CURVE('',#2600,#2600,#2213,.T.);
#3176=EDGE_CURVE('',#2601,#2601,#2214,.T.);
#3177=EDGE_CURVE('',#2601,#2600,#1630,.T.);
#3178=EDGE_CURVE('',#2602,#2602,#2215,.T.);
#3179=EDGE_CURVE('',#2602,#2601,#1631,.T.);
#3180=EDGE_CURVE('',#2603,#2603,#2216,.T.);
#3181=EDGE_CURVE('',#2603,#2602,#1632,.T.);
#3182=EDGE_CURVE('',#2604,#2604,#2217,.T.);
#3183=EDGE_CURVE('',#2605,#2605,#2218,.F.);
#3184=EDGE_CURVE('',#2605,#2604,#1633,.T.);
#3185=EDGE_CURVE('',#2606,#2606,#2219,.F.);
#3186=EDGE_CURVE('',#2606,#2605,#1634,.T.);
#3187=EDGE_CURVE('',#2607,#2607,#2220,.T.);
#3188=EDGE_CURVE('',#2607,#2606,#1635,.T.);
#3189=EDGE_CURVE('',#2608,#2609,#1636,.T.);
#3190=EDGE_CURVE('',#2609,#2610,#1637,.T.);
#3191=EDGE_CURVE('',#2610,#2611,#1638,.T.);
#3192=EDGE_CURVE('',#2608,#2611,#1639,.T.);
#3193=EDGE_CURVE('',#2609,#2612,#1640,.T.);
#3194=EDGE_CURVE('',#2612,#2613,#1641,.T.);
#3195=EDGE_CURVE('',#2613,#2610,#1642,.T.);
#3196=EDGE_CURVE('',#2612,#2614,#1643,.T.);
#3197=EDGE_CURVE('',#2614,#2615,#1644,.T.);
#3198=EDGE_CURVE('',#2615,#2613,#1645,.T.);
#3199=EDGE_CURVE('',#2614,#2616,#1646,.T.);
#3200=EDGE_CURVE('',#2616,#2617,#1647,.T.);
#3201=EDGE_CURVE('',#2617,#2615,#1648,.T.);
#3202=EDGE_CURVE('',#2616,#2618,#1649,.T.);
#3203=EDGE_CURVE('',#2618,#2619,#1650,.T.);
#3204=EDGE_CURVE('',#2619,#2617,#1651,.T.);
#3205=EDGE_CURVE('',#2618,#2608,#1652,.T.);
#3206=EDGE_CURVE('',#2611,#2619,#1653,.T.);
#3207=ORIENTED_EDGE('',*,*,#2620,.F.);
#3208=ORIENTED_EDGE('',*,*,#2621,.T.);
#3209=ORIENTED_EDGE('',*,*,#2622,.F.);
#3210=ORIENTED_EDGE('',*,*,#2621,.F.);
#3211=ORIENTED_EDGE('',*,*,#2623,.F.);
#3212=ORIENTED_EDGE('',*,*,#2624,.T.);
#3213=ORIENTED_EDGE('',*,*,#2625,.F.);
#3214=ORIENTED_EDGE('',*,*,#2624,.F.);
#3215=ORIENTED_EDGE('',*,*,#2626,.F.);
#3216=ORIENTED_EDGE('',*,*,#2627,.T.);
#3217=ORIENTED_EDGE('',*,*,#2628,.F.);
#3218=ORIENTED_EDGE('',*,*,#2627,.F.);
#3219=ORIENTED_EDGE('',*,*,#2629,.F.);
#3220=ORIENTED_EDGE('',*,*,#2630,.T.);
#3221=ORIENTED_EDGE('',*,*,#2631,.F.);
#3222=ORIENTED_EDGE('',*,*,#2630,.F.);
#3223=ORIENTED_EDGE('',*,*,#2632,.T.);
#3224=ORIENTED_EDGE('',*,*,#2633,.T.);
#3225=ORIENTED_EDGE('',*,*,#2634,.F.);
#3226=ORIENTED_EDGE('',*,*,#2635,.F.);
#3227=ORIENTED_EDGE('',*,*,#2636,.T.);
#3228=ORIENTED_EDGE('',*,*,#2635,.T.);
#3229=ORIENTED_EDGE('',*,*,#2637,.F.);
#3230=ORIENTED_EDGE('',*,*,#2638,.F.);
#3231=ORIENTED_EDGE('',*,*,#2639,.T.);
#3232=ORIENTED_EDGE('',*,*,#2638,.T.);
#3233=ORIENTED_EDGE('',*,*,#2640,.F.);
#3234=ORIENTED_EDGE('',*,*,#2641,.F.);
#3235=ORIENTED_EDGE('',*,*,#2642,.T.);
#3236=ORIENTED_EDGE('',*,*,#2641,.T.);
#3237=ORIENTED_EDGE('',*,*,#2643,.F.);
#3238=ORIENTED_EDGE('',*,*,#2633,.F.);
#3239=ORIENTED_EDGE('',*,*,#2643,.T.);
#3240=ORIENTED_EDGE('',*,*,#2640,.T.);
#3241=ORIENTED_EDGE('',*,*,#2637,.T.);
#3242=ORIENTED_EDGE('',*,*,#2634,.T.);
#3243=ORIENTED_EDGE('',*,*,#2622,.T.);
#3244=ORIENTED_EDGE('',*,*,#2625,.T.);
#3245=ORIENTED_EDGE('',*,*,#2628,.T.);
#3246=ORIENTED_EDGE('',*,*,#2631,.T.);
#3247=ORIENTED_EDGE('',*,*,#2642,.F.);
#3248=ORIENTED_EDGE('',*,*,#2632,.F.);
#3249=ORIENTED_EDGE('',*,*,#2636,.F.);
#3250=ORIENTED_EDGE('',*,*,#2639,.F.);
#3251=ORIENTED_EDGE('',*,*,#2620,.T.);
#3252=ORIENTED_EDGE('',*,*,#2623,.T.);
#3253=ORIENTED_EDGE('',*,*,#2626,.T.);
#3254=ORIENTED_EDGE('',*,*,#2629,.T.);
#3255=ORIENTED_EDGE('',*,*,#2644,.T.);
#3256=ORIENTED_EDGE('',*,*,#2645,.T.);
#3257=ORIENTED_EDGE('',*,*,#2646,.F.);
#3258=ORIENTED_EDGE('',*,*,#2647,.F.);
#3259=ORIENTED_EDGE('',*,*,#2648,.T.);
#3260=ORIENTED_EDGE('',*,*,#2647,.T.);
#3261=ORIENTED_EDGE('',*,*,#2649,.F.);
#3262=ORIENTED_EDGE('',*,*,#2650,.F.);
#3263=ORIENTED_EDGE('',*,*,#2651,.T.);
#3264=ORIENTED_EDGE('',*,*,#2650,.T.);
#3265=ORIENTED_EDGE('',*,*,#2652,.F.);
#3266=ORIENTED_EDGE('',*,*,#2653,.F.);
#3267=ORIENTED_EDGE('',*,*,#2654,.T.);
#3268=ORIENTED_EDGE('',*,*,#2653,.T.);
#3269=ORIENTED_EDGE('',*,*,#2655,.F.);
#3270=ORIENTED_EDGE('',*,*,#2645,.F.);
#3271=ORIENTED_EDGE('',*,*,#2655,.T.);
#3272=ORIENTED_EDGE('',*,*,#2652,.T.);
#3273=ORIENTED_EDGE('',*,*,#2649,.T.);
#3274=ORIENTED_EDGE('',*,*,#2646,.T.);
#3275=ORIENTED_EDGE('',*,*,#2654,.F.);
#3276=ORIENTED_EDGE('',*,*,#2644,.F.);
#3277=ORIENTED_EDGE('',*,*,#2648,.F.);
#3278=ORIENTED_EDGE('',*,*,#2651,.F.);
#3279=ORIENTED_EDGE('',*,*,#2656,.T.);
#3280=ORIENTED_EDGE('',*,*,#2657,.T.);
#3281=ORIENTED_EDGE('',*,*,#2658,.F.);
#3282=ORIENTED_EDGE('',*,*,#2659,.F.);
#3283=ORIENTED_EDGE('',*,*,#2660,.T.);
#3284=ORIENTED_EDGE('',*,*,#2659,.T.);
#3285=ORIENTED_EDGE('',*,*,#2661,.F.);
#3286=ORIENTED_EDGE('',*,*,#2662,.F.);
#3287=ORIENTED_EDGE('',*,*,#2663,.T.);
#3288=ORIENTED_EDGE('',*,*,#2662,.T.);
#3289=ORIENTED_EDGE('',*,*,#2664,.F.);
#3290=ORIENTED_EDGE('',*,*,#2665,.F.);
#3291=ORIENTED_EDGE('',*,*,#2666,.T.);
#3292=ORIENTED_EDGE('',*,*,#2665,.T.);
#3293=ORIENTED_EDGE('',*,*,#2667,.F.);
#3294=ORIENTED_EDGE('',*,*,#2657,.F.);
#3295=ORIENTED_EDGE('',*,*,#2667,.T.);
#3296=ORIENTED_EDGE('',*,*,#2664,.T.);
#3297=ORIENTED_EDGE('',*,*,#2661,.T.);
#3298=ORIENTED_EDGE('',*,*,#2658,.T.);
#3299=ORIENTED_EDGE('',*,*,#2666,.F.);
#3300=ORIENTED_EDGE('',*,*,#2656,.F.);
#3301=ORIENTED_EDGE('',*,*,#2660,.F.);
#3302=ORIENTED_EDGE('',*,*,#2663,.F.);
#3303=ORIENTED_EDGE('',*,*,#2668,.T.);
#3304=ORIENTED_EDGE('',*,*,#2669,.T.);
#3305=ORIENTED_EDGE('',*,*,#2670,.F.);
#3306=ORIENTED_EDGE('',*,*,#2671,.F.);
#3307=ORIENTED_EDGE('',*,*,#2672,.T.);
#3308=ORIENTED_EDGE('',*,*,#2671,.T.);
#3309=ORIENTED_EDGE('',*,*,#2673,.F.);
#3310=ORIENTED_EDGE('',*,*,#2674,.F.);
#3311=ORIENTED_EDGE('',*,*,#2675,.T.);
#3312=ORIENTED_EDGE('',*,*,#2674,.T.);
#3313=ORIENTED_EDGE('',*,*,#2676,.F.);
#3314=ORIENTED_EDGE('',*,*,#2677,.F.);
#3315=ORIENTED_EDGE('',*,*,#2678,.T.);
#3316=ORIENTED_EDGE('',*,*,#2677,.T.);
#3317=ORIENTED_EDGE('',*,*,#2679,.F.);
#3318=ORIENTED_EDGE('',*,*,#2669,.F.);
#3319=ORIENTED_EDGE('',*,*,#2679,.T.);
#3320=ORIENTED_EDGE('',*,*,#2676,.T.);
#3321=ORIENTED_EDGE('',*,*,#2673,.T.);
#3322=ORIENTED_EDGE('',*,*,#2670,.T.);
#3323=ORIENTED_EDGE('',*,*,#2678,.F.);
#3324=ORIENTED_EDGE('',*,*,#2668,.F.);
#3325=ORIENTED_EDGE('',*,*,#2672,.F.);
#3326=ORIENTED_EDGE('',*,*,#2675,.F.);
#3327=ORIENTED_EDGE('',*,*,#2680,.F.);
#3328=ORIENTED_EDGE('',*,*,#2681,.T.);
#3329=ORIENTED_EDGE('',*,*,#2682,.F.);
#3330=ORIENTED_EDGE('',*,*,#2681,.F.);
#3331=ORIENTED_EDGE('',*,*,#2683,.F.);
#3332=ORIENTED_EDGE('',*,*,#2684,.T.);
#3333=ORIENTED_EDGE('',*,*,#2685,.F.);
#3334=ORIENTED_EDGE('',*,*,#2684,.F.);
#3335=ORIENTED_EDGE('',*,*,#2686,.F.);
#3336=ORIENTED_EDGE('',*,*,#2687,.T.);
#3337=ORIENTED_EDGE('',*,*,#2688,.F.);
#3338=ORIENTED_EDGE('',*,*,#2687,.F.);
#3339=ORIENTED_EDGE('',*,*,#2689,.F.);
#3340=ORIENTED_EDGE('',*,*,#2690,.T.);
#3341=ORIENTED_EDGE('',*,*,#2691,.F.);
#3342=ORIENTED_EDGE('',*,*,#2690,.F.);
#3343=ORIENTED_EDGE('',*,*,#2692,.T.);
#3344=ORIENTED_EDGE('',*,*,#2693,.T.);
#3345=ORIENTED_EDGE('',*,*,#2694,.F.);
#3346=ORIENTED_EDGE('',*,*,#2695,.F.);
#3347=ORIENTED_EDGE('',*,*,#2696,.T.);
#3348=ORIENTED_EDGE('',*,*,#2695,.T.);
#3349=ORIENTED_EDGE('',*,*,#2697,.F.);
#3350=ORIENTED_EDGE('',*,*,#2698,.F.);
#3351=ORIENTED_EDGE('',*,*,#2699,.T.);
#3352=ORIENTED_EDGE('',*,*,#2698,.T.);
#3353=ORIENTED_EDGE('',*,*,#2700,.F.);
#3354=ORIENTED_EDGE('',*,*,#2701,.F.);
#3355=ORIENTED_EDGE('',*,*,#2702,.T.);
#3356=ORIENTED_EDGE('',*,*,#2701,.T.);
#3357=ORIENTED_EDGE('',*,*,#2703,.F.);
#3358=ORIENTED_EDGE('',*,*,#2693,.F.);
#3359=ORIENTED_EDGE('',*,*,#2703,.T.);
#3360=ORIENTED_EDGE('',*,*,#2700,.T.);
#3361=ORIENTED_EDGE('',*,*,#2697,.T.);
#3362=ORIENTED_EDGE('',*,*,#2694,.T.);
#3363=ORIENTED_EDGE('',*,*,#2682,.T.);
#3364=ORIENTED_EDGE('',*,*,#2685,.T.);
#3365=ORIENTED_EDGE('',*,*,#2688,.T.);
#3366=ORIENTED_EDGE('',*,*,#2691,.T.);
#3367=ORIENTED_EDGE('',*,*,#2702,.F.);
#3368=ORIENTED_EDGE('',*,*,#2692,.F.);
#3369=ORIENTED_EDGE('',*,*,#2696,.F.);
#3370=ORIENTED_EDGE('',*,*,#2699,.F.);
#3371=ORIENTED_EDGE('',*,*,#2680,.T.);
#3372=ORIENTED_EDGE('',*,*,#2683,.T.);
#3373=ORIENTED_EDGE('',*,*,#2686,.T.);
#3374=ORIENTED_EDGE('',*,*,#2689,.T.);
#3375=ORIENTED_EDGE('',*,*,#2704,.F.);
#3376=ORIENTED_EDGE('',*,*,#2705,.T.);
#3377=ORIENTED_EDGE('',*,*,#2706,.F.);
#3378=ORIENTED_EDGE('',*,*,#2705,.F.);
#3379=ORIENTED_EDGE('',*,*,#2707,.F.);
#3380=ORIENTED_EDGE('',*,*,#2708,.T.);
#3381=ORIENTED_EDGE('',*,*,#2709,.F.);
#3382=ORIENTED_EDGE('',*,*,#2708,.F.);
#3383=ORIENTED_EDGE('',*,*,#2710,.F.);
#3384=ORIENTED_EDGE('',*,*,#2711,.T.);
#3385=ORIENTED_EDGE('',*,*,#2712,.F.);
#3386=ORIENTED_EDGE('',*,*,#2711,.F.);
#3387=ORIENTED_EDGE('',*,*,#2713,.F.);
#3388=ORIENTED_EDGE('',*,*,#2714,.T.);
#3389=ORIENTED_EDGE('',*,*,#2715,.F.);
#3390=ORIENTED_EDGE('',*,*,#2714,.F.);
#3391=ORIENTED_EDGE('',*,*,#2716,.T.);
#3392=ORIENTED_EDGE('',*,*,#2717,.T.);
#3393=ORIENTED_EDGE('',*,*,#2718,.F.);
#3394=ORIENTED_EDGE('',*,*,#2719,.F.);
#3395=ORIENTED_EDGE('',*,*,#2706,.T.);
#3396=ORIENTED_EDGE('',*,*,#2709,.T.);
#3397=ORIENTED_EDGE('',*,*,#2712,.T.);
#3398=ORIENTED_EDGE('',*,*,#2715,.T.);
#3399=ORIENTED_EDGE('',*,*,#2720,.T.);
#3400=ORIENTED_EDGE('',*,*,#2719,.T.);
#3401=ORIENTED_EDGE('',*,*,#2721,.F.);
#3402=ORIENTED_EDGE('',*,*,#2722,.F.);
#3403=ORIENTED_EDGE('',*,*,#2723,.T.);
#3404=ORIENTED_EDGE('',*,*,#2722,.T.);
#3405=ORIENTED_EDGE('',*,*,#2724,.F.);
#3406=ORIENTED_EDGE('',*,*,#2725,.F.);
#3407=ORIENTED_EDGE('',*,*,#2704,.T.);
#3408=ORIENTED_EDGE('',*,*,#2707,.T.);
#3409=ORIENTED_EDGE('',*,*,#2710,.T.);
#3410=ORIENTED_EDGE('',*,*,#2713,.T.);
#3411=ORIENTED_EDGE('',*,*,#2726,.T.);
#3412=ORIENTED_EDGE('',*,*,#2725,.T.);
#3413=ORIENTED_EDGE('',*,*,#2727,.F.);
#3414=ORIENTED_EDGE('',*,*,#2717,.F.);
#3415=ORIENTED_EDGE('',*,*,#2727,.T.);
#3416=ORIENTED_EDGE('',*,*,#2724,.T.);
#3417=ORIENTED_EDGE('',*,*,#2721,.T.);
#3418=ORIENTED_EDGE('',*,*,#2718,.T.);
#3419=ORIENTED_EDGE('',*,*,#2726,.F.);
#3420=ORIENTED_EDGE('',*,*,#2716,.F.);
#3421=ORIENTED_EDGE('',*,*,#2720,.F.);
#3422=ORIENTED_EDGE('',*,*,#2723,.F.);
#3423=ORIENTED_EDGE('',*,*,#2728,.F.);
#3424=ORIENTED_EDGE('',*,*,#2729,.T.);
#3425=ORIENTED_EDGE('',*,*,#2730,.F.);
#3426=ORIENTED_EDGE('',*,*,#2729,.F.);
#3427=ORIENTED_EDGE('',*,*,#2731,.F.);
#3428=ORIENTED_EDGE('',*,*,#2732,.T.);
#3429=ORIENTED_EDGE('',*,*,#2733,.F.);
#3430=ORIENTED_EDGE('',*,*,#2732,.F.);
#3431=ORIENTED_EDGE('',*,*,#2734,.F.);
#3432=ORIENTED_EDGE('',*,*,#2735,.T.);
#3433=ORIENTED_EDGE('',*,*,#2736,.F.);
#3434=ORIENTED_EDGE('',*,*,#2735,.F.);
#3435=ORIENTED_EDGE('',*,*,#2737,.F.);
#3436=ORIENTED_EDGE('',*,*,#2738,.T.);
#3437=ORIENTED_EDGE('',*,*,#2739,.F.);
#3438=ORIENTED_EDGE('',*,*,#2738,.F.);
#3439=ORIENTED_EDGE('',*,*,#2737,.T.);
#3440=ORIENTED_EDGE('',*,*,#2740,.F.);
#3441=ORIENTED_EDGE('',*,*,#2741,.F.);
#3442=ORIENTED_EDGE('',*,*,#2742,.T.);
#3443=ORIENTED_EDGE('',*,*,#2740,.T.);
#3444=ORIENTED_EDGE('',*,*,#2742,.F.);
#3445=ORIENTED_EDGE('',*,*,#2743,.T.);
#3446=ORIENTED_EDGE('',*,*,#2744,.T.);
#3447=ORIENTED_EDGE('',*,*,#2745,.T.);
#3448=ORIENTED_EDGE('',*,*,#2746,.T.);
#3449=ORIENTED_EDGE('',*,*,#2730,.T.);
#3450=ORIENTED_EDGE('',*,*,#2733,.T.);
#3451=ORIENTED_EDGE('',*,*,#2736,.T.);
#3452=ORIENTED_EDGE('',*,*,#2739,.T.);
#3453=ORIENTED_EDGE('',*,*,#2747,.F.);
#3454=ORIENTED_EDGE('',*,*,#2748,.T.);
#3455=ORIENTED_EDGE('',*,*,#2749,.T.);
#3456=ORIENTED_EDGE('',*,*,#2743,.F.);
#3457=ORIENTED_EDGE('',*,*,#2750,.F.);
#3458=ORIENTED_EDGE('',*,*,#2745,.F.);
#3459=ORIENTED_EDGE('',*,*,#2751,.F.);
#3460=ORIENTED_EDGE('',*,*,#2752,.T.);
#3461=ORIENTED_EDGE('',*,*,#2753,.T.);
#3462=ORIENTED_EDGE('',*,*,#2751,.T.);
#3463=ORIENTED_EDGE('',*,*,#2744,.F.);
#3464=ORIENTED_EDGE('',*,*,#2749,.F.);
#3465=ORIENTED_EDGE('',*,*,#2747,.T.);
#3466=ORIENTED_EDGE('',*,*,#2746,.F.);
#3467=ORIENTED_EDGE('',*,*,#2750,.T.);
#3468=ORIENTED_EDGE('',*,*,#2754,.T.);
#3469=ORIENTED_EDGE('',*,*,#2754,.F.);
#3470=ORIENTED_EDGE('',*,*,#2752,.F.);
#3471=ORIENTED_EDGE('',*,*,#2753,.F.);
#3472=ORIENTED_EDGE('',*,*,#2748,.F.);
#3473=ORIENTED_EDGE('',*,*,#2728,.T.);
#3474=ORIENTED_EDGE('',*,*,#2731,.T.);
#3475=ORIENTED_EDGE('',*,*,#2734,.T.);
#3476=ORIENTED_EDGE('',*,*,#2741,.T.);
#3477=ORIENTED_EDGE('',*,*,#2755,.F.);
#3478=ORIENTED_EDGE('',*,*,#2756,.T.);
#3479=ORIENTED_EDGE('',*,*,#2757,.F.);
#3480=ORIENTED_EDGE('',*,*,#2758,.F.);
#3481=ORIENTED_EDGE('',*,*,#2759,.F.);
#3482=ORIENTED_EDGE('',*,*,#2760,.F.);
#3483=ORIENTED_EDGE('',*,*,#2756,.F.);
#3484=ORIENTED_EDGE('',*,*,#2761,.F.);
#3485=ORIENTED_EDGE('',*,*,#2762,.T.);
#3486=ORIENTED_EDGE('',*,*,#2763,.F.);
#3487=ORIENTED_EDGE('',*,*,#2764,.F.);
#3488=ORIENTED_EDGE('',*,*,#2765,.F.);
#3489=ORIENTED_EDGE('',*,*,#2766,.F.);
#3490=ORIENTED_EDGE('',*,*,#2762,.F.);
#3491=ORIENTED_EDGE('',*,*,#2767,.F.);
#3492=ORIENTED_EDGE('',*,*,#2768,.T.);
#3493=ORIENTED_EDGE('',*,*,#2769,.F.);
#3494=ORIENTED_EDGE('',*,*,#2770,.F.);
#3495=ORIENTED_EDGE('',*,*,#2771,.F.);
#3496=ORIENTED_EDGE('',*,*,#2772,.F.);
#3497=ORIENTED_EDGE('',*,*,#2768,.F.);
#3498=ORIENTED_EDGE('',*,*,#2758,.T.);
#3499=ORIENTED_EDGE('',*,*,#2755,.T.);
#3500=ORIENTED_EDGE('',*,*,#2760,.T.);
#3501=ORIENTED_EDGE('',*,*,#2773,.F.);
#3502=ORIENTED_EDGE('',*,*,#2770,.T.);
#3503=ORIENTED_EDGE('',*,*,#2767,.T.);
#3504=ORIENTED_EDGE('',*,*,#2772,.T.);
#3505=ORIENTED_EDGE('',*,*,#2774,.F.);
#3506=ORIENTED_EDGE('',*,*,#2775,.T.);
#3507=ORIENTED_EDGE('',*,*,#2776,.T.);
#3508=ORIENTED_EDGE('',*,*,#2775,.F.);
#3509=ORIENTED_EDGE('',*,*,#2777,.F.);
#3510=ORIENTED_EDGE('',*,*,#2764,.T.);
#3511=ORIENTED_EDGE('',*,*,#2761,.T.);
#3512=ORIENTED_EDGE('',*,*,#2766,.T.);
#3513=ORIENTED_EDGE('',*,*,#2778,.F.);
#3514=ORIENTED_EDGE('',*,*,#2779,.F.);
#3515=ORIENTED_EDGE('',*,*,#2780,.T.);
#3516=ORIENTED_EDGE('',*,*,#2757,.T.);
#3517=ORIENTED_EDGE('',*,*,#2780,.F.);
#3518=ORIENTED_EDGE('',*,*,#2781,.F.);
#3519=ORIENTED_EDGE('',*,*,#2782,.T.);
#3520=ORIENTED_EDGE('',*,*,#2763,.T.);
#3521=ORIENTED_EDGE('',*,*,#2782,.F.);
#3522=ORIENTED_EDGE('',*,*,#2783,.F.);
#3523=ORIENTED_EDGE('',*,*,#2784,.T.);
#3524=ORIENTED_EDGE('',*,*,#2769,.T.);
#3525=ORIENTED_EDGE('',*,*,#2784,.F.);
#3526=ORIENTED_EDGE('',*,*,#2785,.F.);
#3527=ORIENTED_EDGE('',*,*,#2786,.T.);
#3528=ORIENTED_EDGE('',*,*,#2787,.T.);
#3529=ORIENTED_EDGE('',*,*,#2786,.F.);
#3530=ORIENTED_EDGE('',*,*,#2759,.T.);
#3531=ORIENTED_EDGE('',*,*,#2778,.T.);
#3532=ORIENTED_EDGE('',*,*,#2765,.T.);
#3533=ORIENTED_EDGE('',*,*,#2777,.T.);
#3534=ORIENTED_EDGE('',*,*,#2774,.T.);
#3535=ORIENTED_EDGE('',*,*,#2771,.T.);
#3536=ORIENTED_EDGE('',*,*,#2773,.T.);
#3537=ORIENTED_EDGE('',*,*,#2785,.T.);
#3538=ORIENTED_EDGE('',*,*,#2776,.F.);
#3539=ORIENTED_EDGE('',*,*,#2779,.T.);
#3540=ORIENTED_EDGE('',*,*,#2781,.T.);
#3541=ORIENTED_EDGE('',*,*,#2783,.T.);
#3542=ORIENTED_EDGE('',*,*,#2787,.F.);
#3543=ORIENTED_EDGE('',*,*,#2788,.F.);
#3544=ORIENTED_EDGE('',*,*,#2789,.T.);
#3545=ORIENTED_EDGE('',*,*,#2790,.F.);
#3546=ORIENTED_EDGE('',*,*,#2789,.F.);
#3547=ORIENTED_EDGE('',*,*,#2791,.F.);
#3548=ORIENTED_EDGE('',*,*,#2792,.T.);
#3549=ORIENTED_EDGE('',*,*,#2793,.F.);
#3550=ORIENTED_EDGE('',*,*,#2792,.F.);
#3551=ORIENTED_EDGE('',*,*,#2794,.F.);
#3552=ORIENTED_EDGE('',*,*,#2795,.T.);
#3553=ORIENTED_EDGE('',*,*,#2796,.F.);
#3554=ORIENTED_EDGE('',*,*,#2795,.F.);
#3555=ORIENTED_EDGE('',*,*,#2797,.F.);
#3556=ORIENTED_EDGE('',*,*,#2798,.T.);
#3557=ORIENTED_EDGE('',*,*,#2799,.T.);
#3558=ORIENTED_EDGE('',*,*,#2798,.F.);
#3559=ORIENTED_EDGE('',*,*,#2799,.F.);
#3560=ORIENTED_EDGE('',*,*,#2800,.F.);
#3561=ORIENTED_EDGE('',*,*,#2800,.T.);
#3562=ORIENTED_EDGE('',*,*,#2801,.T.);
#3563=ORIENTED_EDGE('',*,*,#2802,.F.);
#3564=ORIENTED_EDGE('',*,*,#2801,.F.);
#3565=ORIENTED_EDGE('',*,*,#2803,.T.);
#3566=ORIENTED_EDGE('',*,*,#2804,.T.);
#3567=ORIENTED_EDGE('',*,*,#2805,.T.);
#3568=ORIENTED_EDGE('',*,*,#2806,.T.);
#3569=ORIENTED_EDGE('',*,*,#2790,.T.);
#3570=ORIENTED_EDGE('',*,*,#2793,.T.);
#3571=ORIENTED_EDGE('',*,*,#2796,.T.);
#3572=ORIENTED_EDGE('',*,*,#2802,.T.);
#3573=ORIENTED_EDGE('',*,*,#2807,.F.);
#3574=ORIENTED_EDGE('',*,*,#2808,.T.);
#3575=ORIENTED_EDGE('',*,*,#2809,.T.);
#3576=ORIENTED_EDGE('',*,*,#2803,.F.);
#3577=ORIENTED_EDGE('',*,*,#2810,.F.);
#3578=ORIENTED_EDGE('',*,*,#2805,.F.);
#3579=ORIENTED_EDGE('',*,*,#2811,.F.);
#3580=ORIENTED_EDGE('',*,*,#2812,.T.);
#3581=ORIENTED_EDGE('',*,*,#2813,.T.);
#3582=ORIENTED_EDGE('',*,*,#2811,.T.);
#3583=ORIENTED_EDGE('',*,*,#2804,.F.);
#3584=ORIENTED_EDGE('',*,*,#2809,.F.);
#3585=ORIENTED_EDGE('',*,*,#2807,.T.);
#3586=ORIENTED_EDGE('',*,*,#2806,.F.);
#3587=ORIENTED_EDGE('',*,*,#2810,.T.);
#3588=ORIENTED_EDGE('',*,*,#2814,.T.);
#3589=ORIENTED_EDGE('',*,*,#2814,.F.);
#3590=ORIENTED_EDGE('',*,*,#2812,.F.);
#3591=ORIENTED_EDGE('',*,*,#2813,.F.);
#3592=ORIENTED_EDGE('',*,*,#2808,.F.);
#3593=ORIENTED_EDGE('',*,*,#2788,.T.);
#3594=ORIENTED_EDGE('',*,*,#2791,.T.);
#3595=ORIENTED_EDGE('',*,*,#2794,.T.);
#3596=ORIENTED_EDGE('',*,*,#2797,.T.);
#3597=ORIENTED_EDGE('',*,*,#2815,.F.);
#3598=ORIENTED_EDGE('',*,*,#2816,.T.);
#3599=ORIENTED_EDGE('',*,*,#2817,.F.);
#3600=ORIENTED_EDGE('',*,*,#2818,.F.);
#3601=ORIENTED_EDGE('',*,*,#2819,.F.);
#3602=ORIENTED_EDGE('',*,*,#2816,.F.);
#3603=ORIENTED_EDGE('',*,*,#2820,.F.);
#3604=ORIENTED_EDGE('',*,*,#2821,.F.);
#3605=ORIENTED_EDGE('',*,*,#2822,.T.);
#3606=ORIENTED_EDGE('',*,*,#2823,.F.);
#3607=ORIENTED_EDGE('',*,*,#2824,.F.);
#3608=ORIENTED_EDGE('',*,*,#2825,.F.);
#3609=ORIENTED_EDGE('',*,*,#2822,.F.);
#3610=ORIENTED_EDGE('',*,*,#2826,.F.);
#3611=ORIENTED_EDGE('',*,*,#2827,.F.);
#3612=ORIENTED_EDGE('',*,*,#2828,.T.);
#3613=ORIENTED_EDGE('',*,*,#2829,.F.);
#3614=ORIENTED_EDGE('',*,*,#2830,.F.);
#3615=ORIENTED_EDGE('',*,*,#2831,.F.);
#3616=ORIENTED_EDGE('',*,*,#2828,.F.);
#3617=ORIENTED_EDGE('',*,*,#2832,.F.);
#3618=ORIENTED_EDGE('',*,*,#2818,.T.);
#3619=ORIENTED_EDGE('',*,*,#2833,.F.);
#3620=ORIENTED_EDGE('',*,*,#2830,.T.);
#3621=ORIENTED_EDGE('',*,*,#2834,.F.);
#3622=ORIENTED_EDGE('',*,*,#2835,.F.);
#3623=ORIENTED_EDGE('',*,*,#2824,.T.);
#3624=ORIENTED_EDGE('',*,*,#2836,.F.);
#3625=ORIENTED_EDGE('',*,*,#2837,.F.);
#3626=ORIENTED_EDGE('',*,*,#2820,.T.);
#3627=ORIENTED_EDGE('',*,*,#2838,.T.);
#3628=ORIENTED_EDGE('',*,*,#2839,.F.);
#3629=ORIENTED_EDGE('',*,*,#2838,.F.);
#3630=ORIENTED_EDGE('',*,*,#2826,.T.);
#3631=ORIENTED_EDGE('',*,*,#2840,.T.);
#3632=ORIENTED_EDGE('',*,*,#2841,.F.);
#3633=ORIENTED_EDGE('',*,*,#2840,.F.);
#3634=ORIENTED_EDGE('',*,*,#2832,.T.);
#3635=ORIENTED_EDGE('',*,*,#2842,.T.);
#3636=ORIENTED_EDGE('',*,*,#2843,.F.);
#3637=ORIENTED_EDGE('',*,*,#2842,.F.);
#3638=ORIENTED_EDGE('',*,*,#2844,.F.);
#3639=ORIENTED_EDGE('',*,*,#2845,.T.);
#3640=ORIENTED_EDGE('',*,*,#2837,.T.);
#3641=ORIENTED_EDGE('',*,*,#2845,.F.);
#3642=ORIENTED_EDGE('',*,*,#2846,.F.);
#3643=ORIENTED_EDGE('',*,*,#2847,.T.);
#3644=ORIENTED_EDGE('',*,*,#2834,.T.);
#3645=ORIENTED_EDGE('',*,*,#2829,.T.);
#3646=ORIENTED_EDGE('',*,*,#2831,.T.);
#3647=ORIENTED_EDGE('',*,*,#2827,.T.);
#3648=ORIENTED_EDGE('',*,*,#2833,.T.);
#3649=ORIENTED_EDGE('',*,*,#2817,.T.);
#3650=ORIENTED_EDGE('',*,*,#2819,.T.);
#3651=ORIENTED_EDGE('',*,*,#2815,.T.);
#3652=ORIENTED_EDGE('',*,*,#2836,.T.);
#3653=ORIENTED_EDGE('',*,*,#2823,.T.);
#3654=ORIENTED_EDGE('',*,*,#2825,.T.);
#3655=ORIENTED_EDGE('',*,*,#2821,.T.);
#3656=ORIENTED_EDGE('',*,*,#2835,.T.);
#3657=ORIENTED_EDGE('',*,*,#2847,.F.);
#3658=ORIENTED_EDGE('',*,*,#2846,.T.);
#3659=ORIENTED_EDGE('',*,*,#2839,.T.);
#3660=ORIENTED_EDGE('',*,*,#2841,.T.);
#3661=ORIENTED_EDGE('',*,*,#2843,.T.);
#3662=ORIENTED_EDGE('',*,*,#2844,.T.);
#3663=ORIENTED_EDGE('',*,*,#2848,.F.);
#3664=ORIENTED_EDGE('',*,*,#2849,.T.);
#3665=ORIENTED_EDGE('',*,*,#2850,.F.);
#3666=ORIENTED_EDGE('',*,*,#2849,.F.);
#3667=ORIENTED_EDGE('',*,*,#2851,.F.);
#3668=ORIENTED_EDGE('',*,*,#2852,.T.);
#3669=ORIENTED_EDGE('',*,*,#2853,.F.);
#3670=ORIENTED_EDGE('',*,*,#2854,.F.);
#3671=ORIENTED_EDGE('',*,*,#2855,.T.);
#3672=ORIENTED_EDGE('',*,*,#2853,.T.);
#3673=ORIENTED_EDGE('',*,*,#2856,.T.);
#3674=ORIENTED_EDGE('',*,*,#2857,.T.);
#3675=ORIENTED_EDGE('',*,*,#2858,.F.);
#3676=ORIENTED_EDGE('',*,*,#2859,.T.);
#3677=ORIENTED_EDGE('',*,*,#2860,.T.);
#3678=ORIENTED_EDGE('',*,*,#2861,.T.);
#3679=ORIENTED_EDGE('',*,*,#2862,.T.);
#3680=ORIENTED_EDGE('',*,*,#2863,.T.);
#3681=ORIENTED_EDGE('',*,*,#2864,.F.);
#3682=ORIENTED_EDGE('',*,*,#2854,.T.);
#3683=ORIENTED_EDGE('',*,*,#2855,.F.);
#3684=ORIENTED_EDGE('',*,*,#2865,.F.);
#3685=ORIENTED_EDGE('',*,*,#2866,.F.);
#3686=ORIENTED_EDGE('',*,*,#2865,.T.);
#3687=ORIENTED_EDGE('',*,*,#2857,.F.);
#3688=ORIENTED_EDGE('',*,*,#2867,.F.);
#3689=ORIENTED_EDGE('',*,*,#2851,.T.);
#3690=ORIENTED_EDGE('',*,*,#2864,.T.);
#3691=ORIENTED_EDGE('',*,*,#2868,.F.);
#3692=ORIENTED_EDGE('',*,*,#2869,.T.);
#3693=ORIENTED_EDGE('',*,*,#2870,.T.);
#3694=ORIENTED_EDGE('',*,*,#2871,.F.);
#3695=ORIENTED_EDGE('',*,*,#2858,.T.);
#3696=ORIENTED_EDGE('',*,*,#2866,.T.);
#3697=ORIENTED_EDGE('',*,*,#2871,.T.);
#3698=ORIENTED_EDGE('',*,*,#2872,.T.);
#3699=ORIENTED_EDGE('',*,*,#2873,.T.);
#3700=ORIENTED_EDGE('',*,*,#2859,.F.);
#3701=ORIENTED_EDGE('',*,*,#2868,.T.);
#3702=ORIENTED_EDGE('',*,*,#2863,.F.);
#3703=ORIENTED_EDGE('',*,*,#2874,.F.);
#3704=ORIENTED_EDGE('',*,*,#2875,.T.);
#3705=ORIENTED_EDGE('',*,*,#2876,.T.);
#3706=ORIENTED_EDGE('',*,*,#2874,.T.);
#3707=ORIENTED_EDGE('',*,*,#2862,.F.);
#3708=ORIENTED_EDGE('',*,*,#2877,.F.);
#3709=ORIENTED_EDGE('',*,*,#2850,.T.);
#3710=ORIENTED_EDGE('',*,*,#2878,.T.);
#3711=ORIENTED_EDGE('',*,*,#2877,.T.);
#3712=ORIENTED_EDGE('',*,*,#2861,.F.);
#3713=ORIENTED_EDGE('',*,*,#2879,.F.);
#3714=ORIENTED_EDGE('',*,*,#2880,.T.);
#3715=ORIENTED_EDGE('',*,*,#2879,.T.);
#3716=ORIENTED_EDGE('',*,*,#2860,.F.);
#3717=ORIENTED_EDGE('',*,*,#2873,.F.);
#3718=ORIENTED_EDGE('',*,*,#2848,.T.);
#3719=ORIENTED_EDGE('',*,*,#2869,.F.);
#3720=ORIENTED_EDGE('',*,*,#2875,.F.);
#3721=ORIENTED_EDGE('',*,*,#2876,.F.);
#3722=ORIENTED_EDGE('',*,*,#2878,.F.);
#3723=ORIENTED_EDGE('',*,*,#2880,.F.);
#3724=ORIENTED_EDGE('',*,*,#2872,.F.);
#3725=ORIENTED_EDGE('',*,*,#2870,.F.);
#3726=ORIENTED_EDGE('',*,*,#2867,.T.);
#3727=ORIENTED_EDGE('',*,*,#2856,.F.);
#3728=ORIENTED_EDGE('',*,*,#2852,.F.);
#3729=ORIENTED_EDGE('',*,*,#2881,.T.);
#3730=ORIENTED_EDGE('',*,*,#2881,.F.);
#3731=ORIENTED_EDGE('',*,*,#2882,.F.);
#3732=ORIENTED_EDGE('',*,*,#2883,.F.);
#3733=ORIENTED_EDGE('',*,*,#2884,.F.);
#3734=ORIENTED_EDGE('',*,*,#2885,.T.);
#3735=ORIENTED_EDGE('',*,*,#2882,.T.);
#3736=ORIENTED_EDGE('',*,*,#2885,.F.);
#3737=ORIENTED_EDGE('',*,*,#2883,.T.);
#3738=ORIENTED_EDGE('',*,*,#2886,.T.);
#3739=ORIENTED_EDGE('',*,*,#2887,.T.);
#3740=ORIENTED_EDGE('',*,*,#2886,.F.);
#3741=ORIENTED_EDGE('',*,*,#2884,.T.);
#3742=ORIENTED_EDGE('',*,*,#2887,.F.);
#3743=ORIENTED_EDGE('',*,*,#2888,.T.);
#3744=ORIENTED_EDGE('',*,*,#2889,.F.);
#3745=ORIENTED_EDGE('',*,*,#2888,.F.);
#3746=ORIENTED_EDGE('',*,*,#2890,.T.);
#3747=ORIENTED_EDGE('',*,*,#2891,.T.);
#3748=ORIENTED_EDGE('',*,*,#2890,.F.);
#3749=ORIENTED_EDGE('',*,*,#2891,.F.);
#3750=ORIENTED_EDGE('',*,*,#2892,.F.);
#3751=ORIENTED_EDGE('',*,*,#2893,.F.);
#3752=ORIENTED_EDGE('',*,*,#2894,.T.);
#3753=ORIENTED_EDGE('',*,*,#2892,.T.);
#3754=ORIENTED_EDGE('',*,*,#2894,.F.);
#3755=ORIENTED_EDGE('',*,*,#2895,.F.);
#3756=ORIENTED_EDGE('',*,*,#2896,.T.);
#3757=ORIENTED_EDGE('',*,*,#2889,.T.);
#3758=ORIENTED_EDGE('',*,*,#2896,.F.);
#3759=ORIENTED_EDGE('',*,*,#2895,.T.);
#3760=ORIENTED_EDGE('',*,*,#2893,.T.);
#3761=ORIENTED_EDGE('',*,*,#2897,.F.);
#3762=ORIENTED_EDGE('',*,*,#2898,.T.);
#3763=ORIENTED_EDGE('',*,*,#2899,.T.);
#3764=ORIENTED_EDGE('',*,*,#2898,.F.);
#3765=ORIENTED_EDGE('',*,*,#2900,.F.);
#3766=ORIENTED_EDGE('',*,*,#2901,.T.);
#3767=ORIENTED_EDGE('',*,*,#2902,.T.);
#3768=ORIENTED_EDGE('',*,*,#2901,.F.);
#3769=ORIENTED_EDGE('',*,*,#2900,.T.);
#3770=ORIENTED_EDGE('',*,*,#2897,.T.);
#3771=ORIENTED_EDGE('',*,*,#2902,.F.);
#3772=ORIENTED_EDGE('',*,*,#2899,.F.);
#3773=ORIENTED_EDGE('',*,*,#2903,.T.);
#3774=ORIENTED_EDGE('',*,*,#2904,.T.);
#3775=ORIENTED_EDGE('',*,*,#2905,.F.);
#3776=ORIENTED_EDGE('',*,*,#2904,.F.);
#3777=ORIENTED_EDGE('',*,*,#2905,.T.);
#3778=ORIENTED_EDGE('',*,*,#2903,.F.);
#3779=ORIENTED_EDGE('',*,*,#2906,.T.);
#3780=ORIENTED_EDGE('',*,*,#2907,.T.);
#3781=ORIENTED_EDGE('',*,*,#2908,.F.);
#3782=ORIENTED_EDGE('',*,*,#2909,.F.);
#3783=ORIENTED_EDGE('',*,*,#2910,.T.);
#3784=ORIENTED_EDGE('',*,*,#2909,.T.);
#3785=ORIENTED_EDGE('',*,*,#2911,.F.);
#3786=ORIENTED_EDGE('',*,*,#2912,.F.);
#3787=ORIENTED_EDGE('',*,*,#2913,.T.);
#3788=ORIENTED_EDGE('',*,*,#2912,.T.);
#3789=ORIENTED_EDGE('',*,*,#2914,.F.);
#3790=ORIENTED_EDGE('',*,*,#2915,.F.);
#3791=ORIENTED_EDGE('',*,*,#2916,.T.);
#3792=ORIENTED_EDGE('',*,*,#2915,.T.);
#3793=ORIENTED_EDGE('',*,*,#2917,.F.);
#3794=ORIENTED_EDGE('',*,*,#2907,.F.);
#3795=ORIENTED_EDGE('',*,*,#2917,.T.);
#3796=ORIENTED_EDGE('',*,*,#2914,.T.);
#3797=ORIENTED_EDGE('',*,*,#2911,.T.);
#3798=ORIENTED_EDGE('',*,*,#2908,.T.);
#3799=ORIENTED_EDGE('',*,*,#2916,.F.);
#3800=ORIENTED_EDGE('',*,*,#2906,.F.);
#3801=ORIENTED_EDGE('',*,*,#2910,.F.);
#3802=ORIENTED_EDGE('',*,*,#2913,.F.);
#3803=ORIENTED_EDGE('',*,*,#2918,.T.);
#3804=ORIENTED_EDGE('',*,*,#2919,.T.);
#3805=ORIENTED_EDGE('',*,*,#2920,.F.);
#3806=ORIENTED_EDGE('',*,*,#2921,.F.);
#3807=ORIENTED_EDGE('',*,*,#2922,.T.);
#3808=ORIENTED_EDGE('',*,*,#2921,.T.);
#3809=ORIENTED_EDGE('',*,*,#2923,.F.);
#3810=ORIENTED_EDGE('',*,*,#2924,.F.);
#3811=ORIENTED_EDGE('',*,*,#2925,.T.);
#3812=ORIENTED_EDGE('',*,*,#2924,.T.);
#3813=ORIENTED_EDGE('',*,*,#2926,.F.);
#3814=ORIENTED_EDGE('',*,*,#2927,.F.);
#3815=ORIENTED_EDGE('',*,*,#2928,.T.);
#3816=ORIENTED_EDGE('',*,*,#2927,.T.);
#3817=ORIENTED_EDGE('',*,*,#2929,.F.);
#3818=ORIENTED_EDGE('',*,*,#2919,.F.);
#3819=ORIENTED_EDGE('',*,*,#2929,.T.);
#3820=ORIENTED_EDGE('',*,*,#2926,.T.);
#3821=ORIENTED_EDGE('',*,*,#2923,.T.);
#3822=ORIENTED_EDGE('',*,*,#2920,.T.);
#3823=ORIENTED_EDGE('',*,*,#2928,.F.);
#3824=ORIENTED_EDGE('',*,*,#2918,.F.);
#3825=ORIENTED_EDGE('',*,*,#2922,.F.);
#3826=ORIENTED_EDGE('',*,*,#2925,.F.);
#3827=ORIENTED_EDGE('',*,*,#2930,.F.);
#3828=ORIENTED_EDGE('',*,*,#2931,.T.);
#3829=ORIENTED_EDGE('',*,*,#2932,.T.);
#3830=ORIENTED_EDGE('',*,*,#2931,.F.);
#3831=ORIENTED_EDGE('',*,*,#2933,.F.);
#3832=ORIENTED_EDGE('',*,*,#2934,.T.);
#3833=ORIENTED_EDGE('',*,*,#2935,.T.);
#3834=ORIENTED_EDGE('',*,*,#2934,.F.);
#3835=ORIENTED_EDGE('',*,*,#2933,.T.);
#3836=ORIENTED_EDGE('',*,*,#2930,.T.);
#3837=ORIENTED_EDGE('',*,*,#2935,.F.);
#3838=ORIENTED_EDGE('',*,*,#2932,.F.);
#3839=ORIENTED_EDGE('',*,*,#2936,.T.);
#3840=ORIENTED_EDGE('',*,*,#2937,.T.);
#3841=ORIENTED_EDGE('',*,*,#2938,.T.);
#3842=ORIENTED_EDGE('',*,*,#2939,.F.);
#3843=ORIENTED_EDGE('',*,*,#2940,.T.);
#3844=ORIENTED_EDGE('',*,*,#2941,.T.);
#3845=ORIENTED_EDGE('',*,*,#2942,.T.);
#3846=ORIENTED_EDGE('',*,*,#2937,.F.);
#3847=ORIENTED_EDGE('',*,*,#2943,.T.);
#3848=ORIENTED_EDGE('',*,*,#2944,.T.);
#3849=ORIENTED_EDGE('',*,*,#2945,.T.);
#3850=ORIENTED_EDGE('',*,*,#2941,.F.);
#3851=ORIENTED_EDGE('',*,*,#2946,.T.);
#3852=ORIENTED_EDGE('',*,*,#2947,.T.);
#3853=ORIENTED_EDGE('',*,*,#2948,.T.);
#3854=ORIENTED_EDGE('',*,*,#2944,.F.);
#3855=ORIENTED_EDGE('',*,*,#2949,.T.);
#3856=ORIENTED_EDGE('',*,*,#2950,.T.);
#3857=ORIENTED_EDGE('',*,*,#2951,.T.);
#3858=ORIENTED_EDGE('',*,*,#2947,.F.);
#3859=ORIENTED_EDGE('',*,*,#2952,.T.);
#3860=ORIENTED_EDGE('',*,*,#2939,.T.);
#3861=ORIENTED_EDGE('',*,*,#2953,.T.);
#3862=ORIENTED_EDGE('',*,*,#2950,.F.);
#3863=ORIENTED_EDGE('',*,*,#2952,.F.);
#3864=ORIENTED_EDGE('',*,*,#2949,.F.);
#3865=ORIENTED_EDGE('',*,*,#2946,.F.);
#3866=ORIENTED_EDGE('',*,*,#2943,.F.);
#3867=ORIENTED_EDGE('',*,*,#2940,.F.);
#3868=ORIENTED_EDGE('',*,*,#2936,.F.);
#3869=ORIENTED_EDGE('',*,*,#2953,.F.);
#3870=ORIENTED_EDGE('',*,*,#2938,.F.);
#3871=ORIENTED_EDGE('',*,*,#2942,.F.);
#3872=ORIENTED_EDGE('',*,*,#2945,.F.);
#3873=ORIENTED_EDGE('',*,*,#2948,.F.);
#3874=ORIENTED_EDGE('',*,*,#2951,.F.);
#3875=ORIENTED_EDGE('',*,*,#2954,.F.);
#3876=ORIENTED_EDGE('',*,*,#2955,.F.);
#3877=ORIENTED_EDGE('',*,*,#2956,.F.);
#3878=ORIENTED_EDGE('',*,*,#2957,.T.);
#3879=ORIENTED_EDGE('',*,*,#2955,.T.);
#3880=ORIENTED_EDGE('',*,*,#2957,.F.);
#3881=ORIENTED_EDGE('',*,*,#2958,.F.);
#3882=ORIENTED_EDGE('',*,*,#2959,.T.);
#3883=ORIENTED_EDGE('',*,*,#2956,.T.);
#3884=ORIENTED_EDGE('',*,*,#2959,.F.);
#3885=ORIENTED_EDGE('',*,*,#2960,.F.);
#3886=ORIENTED_EDGE('',*,*,#2961,.T.);
#3887=ORIENTED_EDGE('',*,*,#2958,.T.);
#3888=ORIENTED_EDGE('',*,*,#2961,.F.);
#3889=ORIENTED_EDGE('',*,*,#2960,.T.);
#3890=ORIENTED_EDGE('',*,*,#2962,.F.);
#3891=ORIENTED_EDGE('',*,*,#2963,.F.);
#3892=ORIENTED_EDGE('',*,*,#2964,.T.);
#3893=ORIENTED_EDGE('',*,*,#2962,.T.);
#3894=ORIENTED_EDGE('',*,*,#2964,.F.);
#3895=ORIENTED_EDGE('',*,*,#2954,.T.);
#3896=ORIENTED_EDGE('',*,*,#2965,.T.);
#3897=ORIENTED_EDGE('',*,*,#2963,.T.);
#3898=ORIENTED_EDGE('',*,*,#2965,.F.);
#3899=ORIENTED_EDGE('',*,*,#2966,.F.);
#3900=ORIENTED_EDGE('',*,*,#2967,.F.);
#3901=ORIENTED_EDGE('',*,*,#2968,.T.);
#3902=ORIENTED_EDGE('',*,*,#2969,.F.);
#3903=ORIENTED_EDGE('',*,*,#2970,.F.);
#3904=ORIENTED_EDGE('',*,*,#2968,.F.);
#3905=ORIENTED_EDGE('',*,*,#2969,.T.);
#3906=ORIENTED_EDGE('',*,*,#2970,.T.);
#3907=ORIENTED_EDGE('',*,*,#2971,.T.);
#3908=ORIENTED_EDGE('',*,*,#2972,.T.);
#3909=ORIENTED_EDGE('',*,*,#2971,.F.);
#3910=ORIENTED_EDGE('',*,*,#2973,.T.);
#3911=ORIENTED_EDGE('',*,*,#2974,.T.);
#3912=ORIENTED_EDGE('',*,*,#2975,.F.);
#3913=ORIENTED_EDGE('',*,*,#2974,.F.);
#3914=ORIENTED_EDGE('',*,*,#2975,.T.);
#3915=ORIENTED_EDGE('',*,*,#2976,.T.);
#3916=ORIENTED_EDGE('',*,*,#2977,.F.);
#3917=ORIENTED_EDGE('',*,*,#2976,.F.);
#3918=ORIENTED_EDGE('',*,*,#2972,.F.);
#3919=ORIENTED_EDGE('',*,*,#2977,.T.);
#3920=ORIENTED_EDGE('',*,*,#2978,.F.);
#3921=ORIENTED_EDGE('',*,*,#2979,.T.);
#3922=ORIENTED_EDGE('',*,*,#2966,.T.);
#3923=ORIENTED_EDGE('',*,*,#2967,.T.);
#3924=ORIENTED_EDGE('',*,*,#2979,.F.);
#3925=ORIENTED_EDGE('',*,*,#2978,.T.);
#3926=ORIENTED_EDGE('',*,*,#2980,.F.);
#3927=ORIENTED_EDGE('',*,*,#2980,.T.);
#3928=ORIENTED_EDGE('',*,*,#2981,.T.);
#3929=ORIENTED_EDGE('',*,*,#2973,.F.);
#3930=ORIENTED_EDGE('',*,*,#2981,.F.);
#3931=ORIENTED_EDGE('',*,*,#2982,.F.);
#3932=ORIENTED_EDGE('',*,*,#2983,.F.);
#3933=ORIENTED_EDGE('',*,*,#2984,.T.);
#3934=ORIENTED_EDGE('',*,*,#2985,.F.);
#3935=ORIENTED_EDGE('',*,*,#2986,.F.);
#3936=ORIENTED_EDGE('',*,*,#2984,.F.);
#3937=ORIENTED_EDGE('',*,*,#2987,.T.);
#3938=ORIENTED_EDGE('',*,*,#2988,.T.);
#3939=ORIENTED_EDGE('',*,*,#2985,.T.);
#3940=ORIENTED_EDGE('',*,*,#2986,.T.);
#3941=ORIENTED_EDGE('',*,*,#2988,.F.);
#3942=ORIENTED_EDGE('',*,*,#2989,.F.);
#3943=ORIENTED_EDGE('',*,*,#2990,.T.);
#3944=ORIENTED_EDGE('',*,*,#2991,.F.);
#3945=ORIENTED_EDGE('',*,*,#2992,.T.);
#3946=ORIENTED_EDGE('',*,*,#2989,.T.);
#3947=ORIENTED_EDGE('',*,*,#2992,.F.);
#3948=ORIENTED_EDGE('',*,*,#2993,.F.);
#3949=ORIENTED_EDGE('',*,*,#2994,.T.);
#3950=ORIENTED_EDGE('',*,*,#2991,.T.);
#3951=ORIENTED_EDGE('',*,*,#2994,.F.);
#3952=ORIENTED_EDGE('',*,*,#2995,.F.);
#3953=ORIENTED_EDGE('',*,*,#2996,.T.);
#3954=ORIENTED_EDGE('',*,*,#2993,.T.);
#3955=ORIENTED_EDGE('',*,*,#2996,.F.);
#3956=ORIENTED_EDGE('',*,*,#2995,.T.);
#3957=ORIENTED_EDGE('',*,*,#2987,.F.);
#3958=ORIENTED_EDGE('',*,*,#2982,.T.);
#3959=ORIENTED_EDGE('',*,*,#2983,.T.);
#3960=ORIENTED_EDGE('',*,*,#2997,.T.);
#3961=ORIENTED_EDGE('',*,*,#2990,.F.);
#3962=ORIENTED_EDGE('',*,*,#2997,.F.);
#3963=ORIENTED_EDGE('',*,*,#2998,.T.);
#3964=ORIENTED_EDGE('',*,*,#2998,.F.);
#3965=ORIENTED_EDGE('',*,*,#2999,.T.);
#3966=ORIENTED_EDGE('',*,*,#2999,.F.);
#3967=ORIENTED_EDGE('',*,*,#3000,.T.);
#3968=ORIENTED_EDGE('',*,*,#3000,.F.);
#3969=ORIENTED_EDGE('',*,*,#3001,.T.);
#3970=ORIENTED_EDGE('',*,*,#3001,.F.);
#3971=ORIENTED_EDGE('',*,*,#3002,.T.);
#3972=ORIENTED_EDGE('',*,*,#3002,.F.);
#3973=ORIENTED_EDGE('',*,*,#3003,.T.);
#3974=ORIENTED_EDGE('',*,*,#3003,.F.);
#3975=ORIENTED_EDGE('',*,*,#3004,.T.);
#3976=ORIENTED_EDGE('',*,*,#3004,.F.);
#3977=ORIENTED_EDGE('',*,*,#3005,.T.);
#3978=ORIENTED_EDGE('',*,*,#3005,.F.);
#3979=ORIENTED_EDGE('',*,*,#3006,.F.);
#3980=ORIENTED_EDGE('',*,*,#3007,.F.);
#3981=ORIENTED_EDGE('',*,*,#3008,.F.);
#3982=ORIENTED_EDGE('',*,*,#3009,.F.);
#3983=ORIENTED_EDGE('',*,*,#3008,.T.);
#3984=ORIENTED_EDGE('',*,*,#3010,.F.);
#3985=ORIENTED_EDGE('',*,*,#3011,.T.);
#3986=ORIENTED_EDGE('',*,*,#3012,.F.);
#3987=ORIENTED_EDGE('',*,*,#3013,.T.);
#3988=ORIENTED_EDGE('',*,*,#3014,.F.);
#3989=ORIENTED_EDGE('',*,*,#3015,.T.);
#3990=ORIENTED_EDGE('',*,*,#3016,.T.);
#3991=ORIENTED_EDGE('',*,*,#3017,.F.);
#3992=ORIENTED_EDGE('',*,*,#3016,.F.);
#3993=ORIENTED_EDGE('',*,*,#3018,.T.);
#3994=ORIENTED_EDGE('',*,*,#3019,.F.);
#3995=ORIENTED_EDGE('',*,*,#3020,.T.);
#3996=ORIENTED_EDGE('',*,*,#3021,.F.);
#3997=ORIENTED_EDGE('',*,*,#3022,.T.);
#3998=ORIENTED_EDGE('',*,*,#3023,.F.);
#3999=ORIENTED_EDGE('',*,*,#3024,.T.);
#4000=ORIENTED_EDGE('',*,*,#3025,.F.);
#4001=ORIENTED_EDGE('',*,*,#3026,.T.);
#4002=ORIENTED_EDGE('',*,*,#3027,.F.);
#4003=ORIENTED_EDGE('',*,*,#3007,.T.);
#4004=ORIENTED_EDGE('',*,*,#3028,.T.);
#4005=ORIENTED_EDGE('',*,*,#3029,.T.);
#4006=ORIENTED_EDGE('',*,*,#3010,.T.);
#4007=ORIENTED_EDGE('',*,*,#3030,.F.);
#4008=ORIENTED_EDGE('',*,*,#3031,.F.);
#4009=ORIENTED_EDGE('',*,*,#3011,.F.);
#4010=ORIENTED_EDGE('',*,*,#3029,.F.);
#4011=ORIENTED_EDGE('',*,*,#3031,.T.);
#4012=ORIENTED_EDGE('',*,*,#3032,.T.);
#4013=ORIENTED_EDGE('',*,*,#3033,.T.);
#4014=ORIENTED_EDGE('',*,*,#3012,.T.);
#4015=ORIENTED_EDGE('',*,*,#3034,.F.);
#4016=ORIENTED_EDGE('',*,*,#3035,.F.);
#4017=ORIENTED_EDGE('',*,*,#3013,.F.);
#4018=ORIENTED_EDGE('',*,*,#3033,.F.);
#4019=ORIENTED_EDGE('',*,*,#3035,.T.);
#4020=ORIENTED_EDGE('',*,*,#3036,.T.);
#4021=ORIENTED_EDGE('',*,*,#3037,.T.);
#4022=ORIENTED_EDGE('',*,*,#3014,.T.);
#4023=ORIENTED_EDGE('',*,*,#3038,.F.);
#4024=ORIENTED_EDGE('',*,*,#3039,.F.);
#4025=ORIENTED_EDGE('',*,*,#3018,.F.);
#4026=ORIENTED_EDGE('',*,*,#3015,.F.);
#4027=ORIENTED_EDGE('',*,*,#3037,.F.);
#4028=ORIENTED_EDGE('',*,*,#3040,.F.);
#4029=ORIENTED_EDGE('',*,*,#3039,.T.);
#4030=ORIENTED_EDGE('',*,*,#3041,.T.);
#4031=ORIENTED_EDGE('',*,*,#3042,.T.);
#4032=ORIENTED_EDGE('',*,*,#3019,.T.);
#4033=ORIENTED_EDGE('',*,*,#3043,.F.);
#4034=ORIENTED_EDGE('',*,*,#3044,.F.);
#4035=ORIENTED_EDGE('',*,*,#3020,.F.);
#4036=ORIENTED_EDGE('',*,*,#3042,.F.);
#4037=ORIENTED_EDGE('',*,*,#3044,.T.);
#4038=ORIENTED_EDGE('',*,*,#3045,.T.);
#4039=ORIENTED_EDGE('',*,*,#3046,.T.);
#4040=ORIENTED_EDGE('',*,*,#3021,.T.);
#4041=ORIENTED_EDGE('',*,*,#3047,.F.);
#4042=ORIENTED_EDGE('',*,*,#3048,.F.);
#4043=ORIENTED_EDGE('',*,*,#3022,.F.);
#4044=ORIENTED_EDGE('',*,*,#3046,.F.);
#4045=ORIENTED_EDGE('',*,*,#3048,.T.);
#4046=ORIENTED_EDGE('',*,*,#3049,.T.);
#4047=ORIENTED_EDGE('',*,*,#3050,.T.);
#4048=ORIENTED_EDGE('',*,*,#3023,.T.);
#4049=ORIENTED_EDGE('',*,*,#3024,.F.);
#4050=ORIENTED_EDGE('',*,*,#3050,.F.);
#4051=ORIENTED_EDGE('',*,*,#3051,.F.);
#4052=ORIENTED_EDGE('',*,*,#3052,.F.);
#4053=ORIENTED_EDGE('',*,*,#3053,.F.);
#4054=ORIENTED_EDGE('',*,*,#3054,.T.);
#4055=ORIENTED_EDGE('',*,*,#3040,.T.);
#4056=ORIENTED_EDGE('',*,*,#3036,.F.);
#4057=ORIENTED_EDGE('',*,*,#3034,.T.);
#4058=ORIENTED_EDGE('',*,*,#3032,.F.);
#4059=ORIENTED_EDGE('',*,*,#3030,.T.);
#4060=ORIENTED_EDGE('',*,*,#3028,.F.);
#4061=ORIENTED_EDGE('',*,*,#3006,.T.);
#4062=ORIENTED_EDGE('',*,*,#3055,.F.);
#4063=ORIENTED_EDGE('',*,*,#3056,.T.);
#4064=ORIENTED_EDGE('',*,*,#3057,.F.);
#4065=ORIENTED_EDGE('',*,*,#3051,.T.);
#4066=ORIENTED_EDGE('',*,*,#3049,.F.);
#4067=ORIENTED_EDGE('',*,*,#3047,.T.);
#4068=ORIENTED_EDGE('',*,*,#3045,.F.);
#4069=ORIENTED_EDGE('',*,*,#3043,.T.);
#4070=ORIENTED_EDGE('',*,*,#3041,.F.);
#4071=ORIENTED_EDGE('',*,*,#3038,.T.);
#4072=ORIENTED_EDGE('',*,*,#3054,.F.);
#4073=ORIENTED_EDGE('',*,*,#3009,.T.);
#4074=ORIENTED_EDGE('',*,*,#3027,.T.);
#4075=ORIENTED_EDGE('',*,*,#3058,.T.);
#4076=ORIENTED_EDGE('',*,*,#3055,.T.);
#4077=ORIENTED_EDGE('',*,*,#3026,.F.);
#4078=ORIENTED_EDGE('',*,*,#3059,.F.);
#4079=ORIENTED_EDGE('',*,*,#3056,.F.);
#4080=ORIENTED_EDGE('',*,*,#3058,.F.);
#4081=ORIENTED_EDGE('',*,*,#3017,.T.);
#4082=ORIENTED_EDGE('',*,*,#3053,.T.);
#4083=ORIENTED_EDGE('',*,*,#3052,.T.);
#4084=ORIENTED_EDGE('',*,*,#3057,.T.);
#4085=ORIENTED_EDGE('',*,*,#3059,.T.);
#4086=ORIENTED_EDGE('',*,*,#3025,.T.);
#4087=ORIENTED_EDGE('',*,*,#3060,.F.);
#4088=ORIENTED_EDGE('',*,*,#3061,.T.);
#4089=ORIENTED_EDGE('',*,*,#3062,.F.);
#4090=ORIENTED_EDGE('',*,*,#3063,.T.);
#4091=ORIENTED_EDGE('',*,*,#3060,.T.);
#4092=ORIENTED_EDGE('',*,*,#3063,.F.);
#4093=ORIENTED_EDGE('',*,*,#3062,.T.);
#4094=ORIENTED_EDGE('',*,*,#3064,.F.);
#4095=ORIENTED_EDGE('',*,*,#3064,.T.);
#4096=ORIENTED_EDGE('',*,*,#3065,.T.);
#4097=ORIENTED_EDGE('',*,*,#3061,.F.);
#4098=ORIENTED_EDGE('',*,*,#3065,.F.);
#4099=ORIENTED_EDGE('',*,*,#3066,.F.);
#4100=ORIENTED_EDGE('',*,*,#3067,.T.);
#4101=ORIENTED_EDGE('',*,*,#3068,.F.);
#4102=ORIENTED_EDGE('',*,*,#3069,.T.);
#4103=ORIENTED_EDGE('',*,*,#3066,.T.);
#4104=ORIENTED_EDGE('',*,*,#3069,.F.);
#4105=ORIENTED_EDGE('',*,*,#3068,.T.);
#4106=ORIENTED_EDGE('',*,*,#3070,.F.);
#4107=ORIENTED_EDGE('',*,*,#3070,.T.);
#4108=ORIENTED_EDGE('',*,*,#3071,.T.);
#4109=ORIENTED_EDGE('',*,*,#3067,.F.);
#4110=ORIENTED_EDGE('',*,*,#3071,.F.);
#4111=ORIENTED_EDGE('',*,*,#3072,.T.);
#4112=ORIENTED_EDGE('',*,*,#3073,.T.);
#4113=ORIENTED_EDGE('',*,*,#3074,.T.);
#4114=ORIENTED_EDGE('',*,*,#3075,.F.);
#4115=ORIENTED_EDGE('',*,*,#3076,.T.);
#4116=ORIENTED_EDGE('',*,*,#3077,.T.);
#4117=ORIENTED_EDGE('',*,*,#3078,.T.);
#4118=ORIENTED_EDGE('',*,*,#3073,.F.);
#4119=ORIENTED_EDGE('',*,*,#3079,.T.);
#4120=ORIENTED_EDGE('',*,*,#3080,.T.);
#4121=ORIENTED_EDGE('',*,*,#3081,.T.);
#4122=ORIENTED_EDGE('',*,*,#3077,.F.);
#4123=ORIENTED_EDGE('',*,*,#3082,.T.);
#4124=ORIENTED_EDGE('',*,*,#3083,.T.);
#4125=ORIENTED_EDGE('',*,*,#3084,.T.);
#4126=ORIENTED_EDGE('',*,*,#3080,.F.);
#4127=ORIENTED_EDGE('',*,*,#3085,.T.);
#4128=ORIENTED_EDGE('',*,*,#3086,.T.);
#4129=ORIENTED_EDGE('',*,*,#3087,.T.);
#4130=ORIENTED_EDGE('',*,*,#3083,.F.);
#4131=ORIENTED_EDGE('',*,*,#3088,.T.);
#4132=ORIENTED_EDGE('',*,*,#3075,.T.);
#4133=ORIENTED_EDGE('',*,*,#3089,.T.);
#4134=ORIENTED_EDGE('',*,*,#3086,.F.);
#4135=ORIENTED_EDGE('',*,*,#3088,.F.);
#4136=ORIENTED_EDGE('',*,*,#3085,.F.);
#4137=ORIENTED_EDGE('',*,*,#3082,.F.);
#4138=ORIENTED_EDGE('',*,*,#3079,.F.);
#4139=ORIENTED_EDGE('',*,*,#3076,.F.);
#4140=ORIENTED_EDGE('',*,*,#3072,.F.);
#4141=ORIENTED_EDGE('',*,*,#3089,.F.);
#4142=ORIENTED_EDGE('',*,*,#3074,.F.);
#4143=ORIENTED_EDGE('',*,*,#3078,.F.);
#4144=ORIENTED_EDGE('',*,*,#3081,.F.);
#4145=ORIENTED_EDGE('',*,*,#3084,.F.);
#4146=ORIENTED_EDGE('',*,*,#3087,.F.);
#4147=ORIENTED_EDGE('',*,*,#3090,.F.);
#4148=ORIENTED_EDGE('',*,*,#3091,.F.);
#4149=ORIENTED_EDGE('',*,*,#3092,.F.);
#4150=ORIENTED_EDGE('',*,*,#3093,.T.);
#4151=ORIENTED_EDGE('',*,*,#3091,.T.);
#4152=ORIENTED_EDGE('',*,*,#3093,.F.);
#4153=ORIENTED_EDGE('',*,*,#3094,.F.);
#4154=ORIENTED_EDGE('',*,*,#3095,.T.);
#4155=ORIENTED_EDGE('',*,*,#3092,.T.);
#4156=ORIENTED_EDGE('',*,*,#3095,.F.);
#4157=ORIENTED_EDGE('',*,*,#3096,.F.);
#4158=ORIENTED_EDGE('',*,*,#3097,.T.);
#4159=ORIENTED_EDGE('',*,*,#3094,.T.);
#4160=ORIENTED_EDGE('',*,*,#3097,.F.);
#4161=ORIENTED_EDGE('',*,*,#3096,.T.);
#4162=ORIENTED_EDGE('',*,*,#3098,.F.);
#4163=ORIENTED_EDGE('',*,*,#3099,.F.);
#4164=ORIENTED_EDGE('',*,*,#3100,.T.);
#4165=ORIENTED_EDGE('',*,*,#3098,.T.);
#4166=ORIENTED_EDGE('',*,*,#3100,.F.);
#4167=ORIENTED_EDGE('',*,*,#3090,.T.);
#4168=ORIENTED_EDGE('',*,*,#3101,.T.);
#4169=ORIENTED_EDGE('',*,*,#3099,.T.);
#4170=ORIENTED_EDGE('',*,*,#3101,.F.);
#4171=ORIENTED_EDGE('',*,*,#3102,.F.);
#4172=ORIENTED_EDGE('',*,*,#3103,.T.);
#4173=ORIENTED_EDGE('',*,*,#3104,.F.);
#4174=ORIENTED_EDGE('',*,*,#3103,.F.);
#4175=ORIENTED_EDGE('',*,*,#3102,.T.);
#4176=ORIENTED_EDGE('',*,*,#3105,.F.);
#4177=ORIENTED_EDGE('',*,*,#3106,.T.);
#4178=ORIENTED_EDGE('',*,*,#3107,.T.);
#4179=ORIENTED_EDGE('',*,*,#3106,.F.);
#4180=ORIENTED_EDGE('',*,*,#3107,.F.);
#4181=ORIENTED_EDGE('',*,*,#3108,.F.);
#4182=ORIENTED_EDGE('',*,*,#3109,.F.);
#4183=ORIENTED_EDGE('',*,*,#3110,.F.);
#4184=ORIENTED_EDGE('',*,*,#3111,.F.);
#4185=ORIENTED_EDGE('',*,*,#3112,.T.);
#4186=ORIENTED_EDGE('',*,*,#3113,.F.);
#4187=ORIENTED_EDGE('',*,*,#3112,.F.);
#4188=ORIENTED_EDGE('',*,*,#3114,.F.);
#4189=ORIENTED_EDGE('',*,*,#3115,.T.);
#4190=ORIENTED_EDGE('',*,*,#3108,.T.);
#4191=ORIENTED_EDGE('',*,*,#3116,.F.);
#4192=ORIENTED_EDGE('',*,*,#3115,.F.);
#4193=ORIENTED_EDGE('',*,*,#3117,.F.);
#4194=ORIENTED_EDGE('',*,*,#3118,.F.);
#4195=ORIENTED_EDGE('',*,*,#3109,.T.);
#4196=ORIENTED_EDGE('',*,*,#3113,.T.);
#4197=ORIENTED_EDGE('',*,*,#3116,.T.);
#4198=ORIENTED_EDGE('',*,*,#3119,.F.);
#4199=ORIENTED_EDGE('',*,*,#3120,.T.);
#4200=ORIENTED_EDGE('',*,*,#3121,.T.);
#4201=ORIENTED_EDGE('',*,*,#3122,.F.);
#4202=ORIENTED_EDGE('',*,*,#3123,.F.);
#4203=ORIENTED_EDGE('',*,*,#3124,.T.);
#4204=ORIENTED_EDGE('',*,*,#3125,.T.);
#4205=ORIENTED_EDGE('',*,*,#3126,.T.);
#4206=ORIENTED_EDGE('',*,*,#3127,.T.);
#4207=ORIENTED_EDGE('',*,*,#3118,.T.);
#4208=ORIENTED_EDGE('',*,*,#3128,.T.);
#4209=ORIENTED_EDGE('',*,*,#3129,.T.);
#4210=ORIENTED_EDGE('',*,*,#3119,.T.);
#4211=ORIENTED_EDGE('',*,*,#3127,.F.);
#4212=ORIENTED_EDGE('',*,*,#3130,.T.);
#4213=ORIENTED_EDGE('',*,*,#3131,.F.);
#4214=ORIENTED_EDGE('',*,*,#3130,.F.);
#4215=ORIENTED_EDGE('',*,*,#3126,.F.);
#4216=ORIENTED_EDGE('',*,*,#3132,.T.);
#4217=ORIENTED_EDGE('',*,*,#3133,.F.);
#4218=ORIENTED_EDGE('',*,*,#3132,.F.);
#4219=ORIENTED_EDGE('',*,*,#3125,.F.);
#4220=ORIENTED_EDGE('',*,*,#3134,.T.);
#4221=ORIENTED_EDGE('',*,*,#3135,.F.);
#4222=ORIENTED_EDGE('',*,*,#3134,.F.);
#4223=ORIENTED_EDGE('',*,*,#3124,.F.);
#4224=ORIENTED_EDGE('',*,*,#3136,.T.);
#4225=ORIENTED_EDGE('',*,*,#3137,.F.);
#4226=ORIENTED_EDGE('',*,*,#3136,.F.);
#4227=ORIENTED_EDGE('',*,*,#3111,.T.);
#4228=ORIENTED_EDGE('',*,*,#3138,.F.);
#4229=ORIENTED_EDGE('',*,*,#3139,.F.);
#4230=ORIENTED_EDGE('',*,*,#3140,.F.);
#4231=ORIENTED_EDGE('',*,*,#3141,.T.);
#4232=ORIENTED_EDGE('',*,*,#3128,.F.);
#4233=ORIENTED_EDGE('',*,*,#3117,.T.);
#4234=ORIENTED_EDGE('',*,*,#3114,.T.);
#4235=ORIENTED_EDGE('',*,*,#3131,.T.);
#4236=ORIENTED_EDGE('',*,*,#3133,.T.);
#4237=ORIENTED_EDGE('',*,*,#3135,.T.);
#4238=ORIENTED_EDGE('',*,*,#3137,.T.);
#4239=ORIENTED_EDGE('',*,*,#3142,.T.);
#4240=ORIENTED_EDGE('',*,*,#3140,.T.);
#4241=ORIENTED_EDGE('',*,*,#3143,.F.);
#4242=ORIENTED_EDGE('',*,*,#3121,.F.);
#4243=ORIENTED_EDGE('',*,*,#3110,.T.);
#4244=ORIENTED_EDGE('',*,*,#3123,.T.);
#4245=ORIENTED_EDGE('',*,*,#3144,.F.);
#4246=ORIENTED_EDGE('',*,*,#3138,.T.);
#4247=ORIENTED_EDGE('',*,*,#3129,.F.);
#4248=ORIENTED_EDGE('',*,*,#3141,.F.);
#4249=ORIENTED_EDGE('',*,*,#3142,.F.);
#4250=ORIENTED_EDGE('',*,*,#3120,.F.);
#4251=ORIENTED_EDGE('',*,*,#3145,.F.);
#4252=ORIENTED_EDGE('',*,*,#3144,.T.);
#4253=ORIENTED_EDGE('',*,*,#3122,.T.);
#4254=ORIENTED_EDGE('',*,*,#3143,.T.);
#4255=ORIENTED_EDGE('',*,*,#3139,.T.);
#4256=ORIENTED_EDGE('',*,*,#3146,.F.);
#4257=ORIENTED_EDGE('',*,*,#3145,.T.);
#4258=ORIENTED_EDGE('',*,*,#3147,.T.);
#4259=ORIENTED_EDGE('',*,*,#3148,.T.);
#4260=ORIENTED_EDGE('',*,*,#3147,.F.);
#4261=ORIENTED_EDGE('',*,*,#3149,.F.);
#4262=ORIENTED_EDGE('',*,*,#3150,.T.);
#4263=ORIENTED_EDGE('',*,*,#3146,.T.);
#4264=ORIENTED_EDGE('',*,*,#3150,.F.);
#4265=ORIENTED_EDGE('',*,*,#3149,.T.);
#4266=ORIENTED_EDGE('',*,*,#3104,.T.);
#4267=ORIENTED_EDGE('',*,*,#3148,.F.);
#4268=ORIENTED_EDGE('',*,*,#3105,.T.);
#4269=ORIENTED_EDGE('',*,*,#3151,.F.);
#4270=ORIENTED_EDGE('',*,*,#3152,.T.);
#4271=ORIENTED_EDGE('',*,*,#3153,.T.);
#4272=ORIENTED_EDGE('',*,*,#3152,.F.);
#4273=ORIENTED_EDGE('',*,*,#3154,.F.);
#4274=ORIENTED_EDGE('',*,*,#3155,.T.);
#4275=ORIENTED_EDGE('',*,*,#3156,.T.);
#4276=ORIENTED_EDGE('',*,*,#3155,.F.);
#4277=ORIENTED_EDGE('',*,*,#3154,.T.);
#4278=ORIENTED_EDGE('',*,*,#3151,.T.);
#4279=ORIENTED_EDGE('',*,*,#3156,.F.);
#4280=ORIENTED_EDGE('',*,*,#3153,.F.);
#4281=ORIENTED_EDGE('',*,*,#3157,.F.);
#4282=ORIENTED_EDGE('',*,*,#3158,.T.);
#4283=ORIENTED_EDGE('',*,*,#3159,.T.);
#4284=ORIENTED_EDGE('',*,*,#3158,.F.);
#4285=ORIENTED_EDGE('',*,*,#3160,.F.);
#4286=ORIENTED_EDGE('',*,*,#3161,.T.);
#4287=ORIENTED_EDGE('',*,*,#3162,.T.);
#4288=ORIENTED_EDGE('',*,*,#3161,.F.);
#4289=ORIENTED_EDGE('',*,*,#3160,.T.);
#4290=ORIENTED_EDGE('',*,*,#3157,.T.);
#4291=ORIENTED_EDGE('',*,*,#3162,.F.);
#4292=ORIENTED_EDGE('',*,*,#3159,.F.);
#4293=ORIENTED_EDGE('',*,*,#3163,.F.);
#4294=ORIENTED_EDGE('',*,*,#3164,.T.);
#4295=ORIENTED_EDGE('',*,*,#3165,.T.);
#4296=ORIENTED_EDGE('',*,*,#3164,.F.);
#4297=ORIENTED_EDGE('',*,*,#3166,.F.);
#4298=ORIENTED_EDGE('',*,*,#3167,.T.);
#4299=ORIENTED_EDGE('',*,*,#3168,.T.);
#4300=ORIENTED_EDGE('',*,*,#3167,.F.);
#4301=ORIENTED_EDGE('',*,*,#3166,.T.);
#4302=ORIENTED_EDGE('',*,*,#3163,.T.);
#4303=ORIENTED_EDGE('',*,*,#3168,.F.);
#4304=ORIENTED_EDGE('',*,*,#3165,.F.);
#4305=ORIENTED_EDGE('',*,*,#3169,.F.);
#4306=ORIENTED_EDGE('',*,*,#3170,.T.);
#4307=ORIENTED_EDGE('',*,*,#3171,.T.);
#4308=ORIENTED_EDGE('',*,*,#3170,.F.);
#4309=ORIENTED_EDGE('',*,*,#3172,.F.);
#4310=ORIENTED_EDGE('',*,*,#3173,.T.);
#4311=ORIENTED_EDGE('',*,*,#3174,.T.);
#4312=ORIENTED_EDGE('',*,*,#3173,.F.);
#4313=ORIENTED_EDGE('',*,*,#3172,.T.);
#4314=ORIENTED_EDGE('',*,*,#3169,.T.);
#4315=ORIENTED_EDGE('',*,*,#3174,.F.);
#4316=ORIENTED_EDGE('',*,*,#3171,.F.);
#4317=ORIENTED_EDGE('',*,*,#3175,.F.);
#4318=ORIENTED_EDGE('',*,*,#3176,.F.);
#4319=ORIENTED_EDGE('',*,*,#3177,.T.);
#4320=ORIENTED_EDGE('',*,*,#3175,.T.);
#4321=ORIENTED_EDGE('',*,*,#3177,.F.);
#4322=ORIENTED_EDGE('',*,*,#3178,.F.);
#4323=ORIENTED_EDGE('',*,*,#3179,.T.);
#4324=ORIENTED_EDGE('',*,*,#3176,.T.);
#4325=ORIENTED_EDGE('',*,*,#3179,.F.);
#4326=ORIENTED_EDGE('',*,*,#3180,.F.);
#4327=ORIENTED_EDGE('',*,*,#3181,.T.);
#4328=ORIENTED_EDGE('',*,*,#3178,.T.);
#4329=ORIENTED_EDGE('',*,*,#3181,.F.);
#4330=ORIENTED_EDGE('',*,*,#3180,.T.);
#4331=ORIENTED_EDGE('',*,*,#3182,.F.);
#4332=ORIENTED_EDGE('',*,*,#3183,.F.);
#4333=ORIENTED_EDGE('',*,*,#3184,.T.);
#4334=ORIENTED_EDGE('',*,*,#3182,.T.);
#4335=ORIENTED_EDGE('',*,*,#3184,.F.);
#4336=ORIENTED_EDGE('',*,*,#3185,.F.);
#4337=ORIENTED_EDGE('',*,*,#3186,.T.);
#4338=ORIENTED_EDGE('',*,*,#3183,.T.);
#4339=ORIENTED_EDGE('',*,*,#3186,.F.);
#4340=ORIENTED_EDGE('',*,*,#3187,.F.);
#4341=ORIENTED_EDGE('',*,*,#3188,.T.);
#4342=ORIENTED_EDGE('',*,*,#3185,.T.);
#4343=ORIENTED_EDGE('',*,*,#3188,.F.);
#4344=ORIENTED_EDGE('',*,*,#3187,.T.);
#4345=ORIENTED_EDGE('',*,*,#3189,.T.);
#4346=ORIENTED_EDGE('',*,*,#3190,.T.);
#4347=ORIENTED_EDGE('',*,*,#3191,.T.);
#4348=ORIENTED_EDGE('',*,*,#3192,.F.);
#4349=ORIENTED_EDGE('',*,*,#3193,.T.);
#4350=ORIENTED_EDGE('',*,*,#3194,.T.);
#4351=ORIENTED_EDGE('',*,*,#3195,.T.);
#4352=ORIENTED_EDGE('',*,*,#3190,.F.);
#4353=ORIENTED_EDGE('',*,*,#3196,.T.);
#4354=ORIENTED_EDGE('',*,*,#3197,.T.);
#4355=ORIENTED_EDGE('',*,*,#3198,.T.);
#4356=ORIENTED_EDGE('',*,*,#3194,.F.);
#4357=ORIENTED_EDGE('',*,*,#3199,.T.);
#4358=ORIENTED_EDGE('',*,*,#3200,.T.);
#4359=ORIENTED_EDGE('',*,*,#3201,.T.);
#4360=ORIENTED_EDGE('',*,*,#3197,.F.);
#4361=ORIENTED_EDGE('',*,*,#3202,.T.);
#4362=ORIENTED_EDGE('',*,*,#3203,.T.);
#4363=ORIENTED_EDGE('',*,*,#3204,.T.);
#4364=ORIENTED_EDGE('',*,*,#3200,.F.);
#4365=ORIENTED_EDGE('',*,*,#3205,.T.);
#4366=ORIENTED_EDGE('',*,*,#3192,.T.);
#4367=ORIENTED_EDGE('',*,*,#3206,.T.);
#4368=ORIENTED_EDGE('',*,*,#3203,.F.);
#4369=ORIENTED_EDGE('',*,*,#3205,.F.);
#4370=ORIENTED_EDGE('',*,*,#3202,.F.);
#4371=ORIENTED_EDGE('',*,*,#3199,.F.);
#4372=ORIENTED_EDGE('',*,*,#3196,.F.);
#4373=ORIENTED_EDGE('',*,*,#3193,.F.);
#4374=ORIENTED_EDGE('',*,*,#3189,.F.);
#4375=ORIENTED_EDGE('',*,*,#3206,.F.);
#4376=ORIENTED_EDGE('',*,*,#3191,.F.);
#4377=ORIENTED_EDGE('',*,*,#3195,.F.);
#4378=ORIENTED_EDGE('',*,*,#3198,.F.);
#4379=ORIENTED_EDGE('',*,*,#3201,.F.);
#4380=ORIENTED_EDGE('',*,*,#3204,.F.);
#4381=CYLINDRICAL_SURFACE('',#5141,0.25);
#4382=CYLINDRICAL_SURFACE('',#5144,0.25);
#4383=CYLINDRICAL_SURFACE('',#5147,0.25);
#4384=CYLINDRICAL_SURFACE('',#5150,0.25);
#4385=CYLINDRICAL_SURFACE('',#5180,0.33);
#4386=CYLINDRICAL_SURFACE('',#5183,0.33);
#4387=CYLINDRICAL_SURFACE('',#5186,0.33);
#4388=CYLINDRICAL_SURFACE('',#5189,0.33);
#4389=CYLINDRICAL_SURFACE('',#5199,0.33);
#4390=CYLINDRICAL_SURFACE('',#5202,0.33);
#4391=CYLINDRICAL_SURFACE('',#5205,0.33);
#4392=CYLINDRICAL_SURFACE('',#5208,0.33);
#4393=CYLINDRICAL_SURFACE('',#5218,0.165);
#4394=CYLINDRICAL_SURFACE('',#5221,0.165);
#4395=CYLINDRICAL_SURFACE('',#5224,0.165);
#4396=CYLINDRICAL_SURFACE('',#5227,1.5);
#4397=CYLINDRICAL_SURFACE('',#5232,1.02);
#4398=CYLINDRICAL_SURFACE('',#5239,2.1);
#4399=CYLINDRICAL_SURFACE('',#5247,0.375);
#4400=CYLINDRICAL_SURFACE('',#5253,0.375);
#4401=CYLINDRICAL_SURFACE('',#5259,0.375);
#4402=CYLINDRICAL_SURFACE('',#5261,2.1);
#4403=CYLINDRICAL_SURFACE('',#5267,0.225);
#4404=CYLINDRICAL_SURFACE('',#5269,0.225);
#4405=CYLINDRICAL_SURFACE('',#5271,0.225);
#4406=CYLINDRICAL_SURFACE('',#5273,1.02);
#4407=CYLINDRICAL_SURFACE('',#5279,0.165);
#4408=CYLINDRICAL_SURFACE('',#5282,0.165);
#4409=CYLINDRICAL_SURFACE('',#5285,0.165);
#4410=CYLINDRICAL_SURFACE('',#5288,1.5);
#4411=CYLINDRICAL_SURFACE('',#5293,1.02);
#4412=CYLINDRICAL_SURFACE('',#5300,2.1);
#4413=CYLINDRICAL_SURFACE('',#5304,0.375);
#4414=CYLINDRICAL_SURFACE('',#5310,0.375);
#4415=CYLINDRICAL_SURFACE('',#5316,0.375);
#4416=CYLINDRICAL_SURFACE('',#5328,0.225);
#4417=CYLINDRICAL_SURFACE('',#5330,0.225);
#4418=CYLINDRICAL_SURFACE('',#5332,0.225);
#4419=CYLINDRICAL_SURFACE('',#5334,1.02);
#4420=CYLINDRICAL_SURFACE('',#5336,2.1);
#4421=CYLINDRICAL_SURFACE('',#5340,0.31);
#4422=CYLINDRICAL_SURFACE('',#5362,0.29);
#4423=CYLINDRICAL_SURFACE('',#5364,0.1);
#4424=CYLINDRICAL_SURFACE('',#5372,0.6);
#4425=CYLINDRICAL_SURFACE('',#5376,0.11);
#4426=CYLINDRICAL_SURFACE('',#5378,0.31);
#4427=CYLINDRICAL_SURFACE('',#5382,0.1);
#4428=CYLINDRICAL_SURFACE('',#5385,0.6);
#4429=CYLINDRICAL_SURFACE('',#5410,0.32);
#4430=CYLINDRICAL_SURFACE('',#5413,0.6);
#4431=CYLINDRICAL_SURFACE('',#5433,0.5);
#4432=CYLINDRICAL_SURFACE('',#5441,0.2942);
#4433=CYLINDRICAL_SURFACE('',#5450,0.976185);
#4434=CYLINDRICAL_SURFACE('',#5452,0.5);
#4435=CYLINDRICAL_SURFACE('',#5458,0.976185);
#4436=CYLINDRICAL_SURFACE('',#5470,1.023815);
#4437=CYLINDRICAL_SURFACE('',#5477,1.5);
#4438=CYLINDRICAL_SURFACE('',#5482,1.023815);
#4439=CYLINDRICAL_SURFACE('',#5504,1.019052);
#4440=CYLINDRICAL_SURFACE('',#5544,0.980948);
#4441=CYLINDRICAL_SURFACE('',#5558,1.013815);
#4442=CYLINDRICAL_SURFACE('',#5562,0.991185);
#4443=CYLINDRICAL_SURFACE('',#5566,1.013815);
#4444=CYLINDRICAL_SURFACE('',#5570,0.991185);
#4445=CYLINDRICAL_SURFACE('',#5591,0.35);
#4446=CYLINDRICAL_SURFACE('',#5599,0.1954);
#4447=CYLINDRICAL_SURFACE('',#5635,0.165);
#4448=CYLINDRICAL_SURFACE('',#5639,0.165);
#4449=CYLINDRICAL_SURFACE('',#5647,1.8);
#4450=CYLINDRICAL_SURFACE('',#5656,1.);
#4451=CYLINDRICAL_SURFACE('',#5658,0.33);
#4452=CYLINDRICAL_SURFACE('',#5660,0.33);
#4453=CYLINDRICAL_SURFACE('',#5662,0.33);
#4454=CYLINDRICAL_SURFACE('',#5664,0.33);
#4455=CYLINDRICAL_SURFACE('',#5668,1.);
#4456=CYLINDRICAL_SURFACE('',#5674,0.5);
#4457=CYLINDRICAL_SURFACE('',#5676,0.5);
#4458=CYLINDRICAL_SURFACE('',#5681,0.505);
#4459=CYLINDRICAL_SURFACE('',#5684,0.7);
#4460=CYLINDRICAL_SURFACE('',#5690,0.505);
#4461=CYLINDRICAL_SURFACE('',#5693,0.7);
#4462=CYLINDRICAL_SURFACE('',#5699,0.225);
#4463=CYLINDRICAL_SURFACE('',#5702,0.9);
#4464=CYLINDRICAL_SURFACE('',#5708,0.225);
#4465=CYLINDRICAL_SURFACE('',#5711,0.9);
#4466=CYLINDRICAL_SURFACE('',#5721,0.35);
#4467=CYLINDRICAL_SURFACE('',#5729,0.1954);
#4468=ADVANCED_FACE('',(#663),#4381,.F.);
#4469=ADVANCED_FACE('',(#664),#4382,.F.);
#4470=ADVANCED_FACE('',(#665),#4383,.F.);
#4471=ADVANCED_FACE('',(#666),#4384,.F.);
#4472=ADVANCED_FACE('',(#667),#500,.T.);
#4473=ADVANCED_FACE('',(#668),#501,.T.);
#4474=ADVANCED_FACE('',(#669),#502,.T.);
#4475=ADVANCED_FACE('',(#670),#503,.T.);
#4476=ADVANCED_FACE('',(#671,#399,#400,#401,#402),#504,.T.);
#4477=ADVANCED_FACE('',(#672,#403,#404,#405,#406),#505,.F.);
#4478=ADVANCED_FACE('',(#673),#506,.T.);
#4479=ADVANCED_FACE('',(#674),#507,.T.);
#4480=ADVANCED_FACE('',(#675),#508,.T.);
#4481=ADVANCED_FACE('',(#676),#509,.T.);
#4482=ADVANCED_FACE('',(#677),#510,.T.);
#4483=ADVANCED_FACE('',(#678),#511,.F.);
#4484=ADVANCED_FACE('',(#679),#512,.T.);
#4485=ADVANCED_FACE('',(#680),#513,.T.);
#4486=ADVANCED_FACE('',(#681),#514,.T.);
#4487=ADVANCED_FACE('',(#682),#515,.T.);
#4488=ADVANCED_FACE('',(#683),#516,.T.);
#4489=ADVANCED_FACE('',(#684),#517,.F.);
#4490=ADVANCED_FACE('',(#685),#518,.T.);
#4491=ADVANCED_FACE('',(#686),#519,.T.);
#4492=ADVANCED_FACE('',(#687),#520,.T.);
#4493=ADVANCED_FACE('',(#688),#521,.T.);
#4494=ADVANCED_FACE('',(#689),#522,.T.);
#4495=ADVANCED_FACE('',(#690),#523,.F.);
#4496=ADVANCED_FACE('',(#691),#4385,.F.);
#4497=ADVANCED_FACE('',(#692),#4386,.F.);
#4498=ADVANCED_FACE('',(#693),#4387,.F.);
#4499=ADVANCED_FACE('',(#694),#4388,.F.);
#4500=ADVANCED_FACE('',(#695),#524,.T.);
#4501=ADVANCED_FACE('',(#696),#525,.T.);
#4502=ADVANCED_FACE('',(#697),#526,.T.);
#4503=ADVANCED_FACE('',(#698),#527,.T.);
#4504=ADVANCED_FACE('',(#699,#407,#408,#409,#410),#528,.T.);
#4505=ADVANCED_FACE('',(#700,#411,#412,#413,#414),#529,.F.);
#4506=ADVANCED_FACE('',(#701),#4389,.F.);
#4507=ADVANCED_FACE('',(#702),#4390,.F.);
#4508=ADVANCED_FACE('',(#703),#4391,.F.);
#4509=ADVANCED_FACE('',(#704),#4392,.F.);
#4510=ADVANCED_FACE('',(#705,#415,#416,#417,#418),#530,.T.);
#4511=ADVANCED_FACE('',(#706),#531,.T.);
#4512=ADVANCED_FACE('',(#707,#419,#420,#421,#422),#532,.T.);
#4513=ADVANCED_FACE('',(#708),#533,.T.);
#4514=ADVANCED_FACE('',(#709),#534,.T.);
#4515=ADVANCED_FACE('',(#710),#535,.F.);
#4516=ADVANCED_FACE('',(#711),#4393,.F.);
#4517=ADVANCED_FACE('',(#712),#4394,.F.);
#4518=ADVANCED_FACE('',(#713),#4395,.F.);
#4519=ADVANCED_FACE('',(#714),#4396,.F.);
#4520=ADVANCED_FACE('',(#715,#423),#536,.T.);
#4521=ADVANCED_FACE('',(#716),#4397,.F.);
#4522=ADVANCED_FACE('',(#717,#424,#425,#426,#427),#537,.T.);
#4523=ADVANCED_FACE('',(#718),#538,.T.);
#4524=ADVANCED_FACE('',(#719),#539,.T.);
#4525=ADVANCED_FACE('',(#720),#540,.T.);
#4526=ADVANCED_FACE('',(#721),#4398,.T.);
#4527=ADVANCED_FACE('',(#722,#428,#429,#430,#431),#541,.F.);
#4528=ADVANCED_FACE('',(#723,#432),#542,.T.);
#4529=ADVANCED_FACE('',(#724),#4399,.F.);
#4530=ADVANCED_FACE('',(#725,#433),#543,.T.);
#4531=ADVANCED_FACE('',(#726),#4400,.F.);
#4532=ADVANCED_FACE('',(#727,#434),#544,.T.);
#4533=ADVANCED_FACE('',(#728),#4401,.F.);
#4534=ADVANCED_FACE('',(#729),#4402,.T.);
#4535=ADVANCED_FACE('',(#730),#4403,.F.);
#4536=ADVANCED_FACE('',(#731),#4404,.F.);
#4537=ADVANCED_FACE('',(#732),#4405,.F.);
#4538=ADVANCED_FACE('',(#733),#4406,.F.);
#4539=ADVANCED_FACE('',(#734,#435),#545,.T.);
#4540=ADVANCED_FACE('',(#735,#436,#437,#438,#439),#546,.F.);
#4541=ADVANCED_FACE('',(#736),#4407,.F.);
#4542=ADVANCED_FACE('',(#737),#4408,.F.);
#4543=ADVANCED_FACE('',(#738),#4409,.F.);
#4544=ADVANCED_FACE('',(#739),#4410,.F.);
#4545=ADVANCED_FACE('',(#740,#440),#547,.F.);
#4546=ADVANCED_FACE('',(#741),#4411,.F.);
#4547=ADVANCED_FACE('',(#742,#441,#442,#443,#444),#548,.T.);
#4548=ADVANCED_FACE('',(#743),#549,.T.);
#4549=ADVANCED_FACE('',(#744),#550,.T.);
#4550=ADVANCED_FACE('',(#745),#551,.T.);
#4551=ADVANCED_FACE('',(#746),#4412,.T.);
#4552=ADVANCED_FACE('',(#747,#445,#446,#447,#448),#552,.F.);
#4553=ADVANCED_FACE('',(#748),#4413,.F.);
#4554=ADVANCED_FACE('',(#749,#449),#553,.F.);
#4555=ADVANCED_FACE('',(#750),#4414,.F.);
#4556=ADVANCED_FACE('',(#751,#450),#554,.F.);
#4557=ADVANCED_FACE('',(#752),#4415,.F.);
#4558=ADVANCED_FACE('',(#753,#451),#555,.F.);
#4559=ADVANCED_FACE('',(#754,#452),#556,.F.);
#4560=ADVANCED_FACE('',(#755),#4416,.F.);
#4561=ADVANCED_FACE('',(#756),#4417,.F.);
#4562=ADVANCED_FACE('',(#757),#4418,.F.);
#4563=ADVANCED_FACE('',(#758),#4419,.F.);
#4564=ADVANCED_FACE('',(#759),#4420,.T.);
#4565=ADVANCED_FACE('',(#760,#453,#454,#455,#456),#557,.T.);
#4566=ADVANCED_FACE('',(#761),#4421,.F.);
#4567=ADVANCED_FACE('',(#762),#558,.T.);
#4568=ADVANCED_FACE('',(#763),#559,.T.);
#4569=ADVANCED_FACE('',(#764),#560,.T.);
#4570=ADVANCED_FACE('',(#765),#561,.T.);
#4571=ADVANCED_FACE('',(#766),#562,.T.);
#4572=ADVANCED_FACE('',(#767),#563,.F.);
#4573=ADVANCED_FACE('',(#768),#564,.T.);
#4574=ADVANCED_FACE('',(#769),#565,.T.);
#4575=ADVANCED_FACE('',(#770,#457),#566,.T.);
#4576=ADVANCED_FACE('',(#771),#567,.T.);
#4577=ADVANCED_FACE('',(#772,#458),#568,.T.);
#4578=ADVANCED_FACE('',(#773),#569,.F.);
#4579=ADVANCED_FACE('',(#774),#242,.T.);
#4580=ADVANCED_FACE('',(#775,#459),#570,.F.);
#4581=ADVANCED_FACE('',(#776),#4422,.T.);
#4582=ADVANCED_FACE('',(#777),#4423,.T.);
#4583=ADVANCED_FACE('',(#778),#571,.T.);
#4584=ADVANCED_FACE('',(#779),#572,.F.);
#4585=ADVANCED_FACE('',(#780,#460),#573,.T.);
#4586=ADVANCED_FACE('',(#781),#4424,.T.);
#4587=ADVANCED_FACE('',(#782,#461),#574,.F.);
#4588=ADVANCED_FACE('',(#783),#4425,.F.);
#4589=ADVANCED_FACE('',(#784),#4426,.T.);
#4590=ADVANCED_FACE('',(#785,#462),#575,.T.);
#4591=ADVANCED_FACE('',(#786),#4427,.F.);
#4592=ADVANCED_FACE('',(#787),#4428,.T.);
#4593=ADVANCED_FACE('',(#788,#463),#576,.T.);
#4594=ADVANCED_FACE('',(#789,#464),#577,.F.);
#4595=ADVANCED_FACE('',(#790),#241,.T.);
#4596=ADVANCED_FACE('',(#791),#578,.T.);
#4597=ADVANCED_FACE('',(#792),#579,.F.);
#4598=ADVANCED_FACE('',(#793),#580,.T.);
#4599=ADVANCED_FACE('',(#794),#581,.T.);
#4600=ADVANCED_FACE('',(#795),#582,.T.);
#4601=ADVANCED_FACE('',(#796),#583,.T.);
#4602=ADVANCED_FACE('',(#797),#584,.T.);
#4603=ADVANCED_FACE('',(#798),#585,.F.);
#4604=ADVANCED_FACE('',(#799),#586,.T.);
#4605=ADVANCED_FACE('',(#800),#587,.T.);
#4606=ADVANCED_FACE('',(#801),#588,.T.);
#4607=ADVANCED_FACE('',(#802),#589,.T.);
#4608=ADVANCED_FACE('',(#803),#590,.T.);
#4609=ADVANCED_FACE('',(#804),#591,.F.);
#4610=ADVANCED_FACE('',(#805),#4429,.F.);
#4611=ADVANCED_FACE('',(#806),#4430,.T.);
#4612=ADVANCED_FACE('',(#807,#465),#592,.T.);
#4613=ADVANCED_FACE('',(#808,#466),#593,.F.);
#4614=ADVANCED_FACE('',(#809),#594,.F.);
#4615=ADVANCED_FACE('',(#810),#595,.F.);
#4616=ADVANCED_FACE('',(#811),#596,.F.);
#4617=ADVANCED_FACE('',(#812),#597,.F.);
#4618=ADVANCED_FACE('',(#813),#598,.F.);
#4619=ADVANCED_FACE('',(#814),#599,.F.);
#4620=ADVANCED_FACE('',(#815),#600,.F.);
#4621=ADVANCED_FACE('',(#816),#601,.F.);
#4622=ADVANCED_FACE('',(#817),#602,.F.);
#4623=ADVANCED_FACE('',(#818),#603,.T.);
#4624=ADVANCED_FACE('',(#819),#201,.T.);
#4625=ADVANCED_FACE('',(#820),#4431,.T.);
#4626=ADVANCED_FACE('',(#821),#202,.T.);
#4627=ADVANCED_FACE('',(#822,#467),#604,.T.);
#4628=ADVANCED_FACE('',(#823),#203,.T.);
#4629=ADVANCED_FACE('',(#824),#4432,.T.);
#4630=ADVANCED_FACE('',(#825),#199,.F.);
#4631=ADVANCED_FACE('',(#826),#4433,.T.);
#4632=ADVANCED_FACE('',(#827),#4434,.F.);
#4633=ADVANCED_FACE('',(#828),#204,.F.);
#4634=ADVANCED_FACE('',(#829,#468),#605,.T.);
#4635=ADVANCED_FACE('',(#830),#4435,.T.);
#4636=ADVANCED_FACE('',(#831,#469),#606,.T.);
#4637=ADVANCED_FACE('',(#832),#205,.F.);
#4638=ADVANCED_FACE('',(#833),#200,.F.);
#4639=ADVANCED_FACE('',(#834),#4436,.F.);
#4640=ADVANCED_FACE('',(#835,#470),#607,.T.);
#4641=ADVANCED_FACE('',(#836),#206,.T.);
#4642=ADVANCED_FACE('',(#837),#4437,.T.);
#4643=ADVANCED_FACE('',(#838),#207,.T.);
#4644=ADVANCED_FACE('',(#839,#471),#608,.T.);
#4645=ADVANCED_FACE('',(#840),#4438,.F.);
#4646=ADVANCED_FACE('',(#841),#243,.T.);
#4647=ADVANCED_FACE('',(#842),#244,.T.);
#4648=ADVANCED_FACE('',(#843),#245,.T.);
#4649=ADVANCED_FACE('',(#844),#246,.T.);
#4650=ADVANCED_FACE('',(#845),#247,.T.);
#4651=ADVANCED_FACE('',(#846),#248,.T.);
#4652=ADVANCED_FACE('',(#847),#249,.T.);
#4653=ADVANCED_FACE('',(#848),#250,.T.);
#4654=ADVANCED_FACE('',(#849),#251,.F.);
#4655=ADVANCED_FACE('',(#850),#4439,.T.);
#4656=ADVANCED_FACE('',(#851),#609,.T.);
#4657=ADVANCED_FACE('',(#852),#252,.F.);
#4658=ADVANCED_FACE('',(#853),#610,.T.);
#4659=ADVANCED_FACE('',(#854),#253,.F.);
#4660=ADVANCED_FACE('',(#855),#611,.T.);
#4661=ADVANCED_FACE('',(#856),#254,.F.);
#4662=ADVANCED_FACE('',(#857),#612,.T.);
#4663=ADVANCED_FACE('',(#858),#255,.F.);
#4664=ADVANCED_FACE('',(#859),#613,.T.);
#4665=ADVANCED_FACE('',(#860),#256,.F.);
#4666=ADVANCED_FACE('',(#861),#614,.T.);
#4667=ADVANCED_FACE('',(#862),#257,.F.);
#4668=ADVANCED_FACE('',(#863),#4440,.F.);
#4669=ADVANCED_FACE('',(#864),#615,.T.);
#4670=ADVANCED_FACE('',(#865),#258,.F.);
#4671=ADVANCED_FACE('',(#866,#472),#616,.T.);
#4672=ADVANCED_FACE('',(#867),#617,.T.);
#4673=ADVANCED_FACE('',(#868,#473),#618,.T.);
#4674=ADVANCED_FACE('',(#869),#4441,.T.);
#4675=ADVANCED_FACE('',(#870,#474),#619,.T.);
#4676=ADVANCED_FACE('',(#871),#4442,.F.);
#4677=ADVANCED_FACE('',(#872,#475),#620,.T.);
#4678=ADVANCED_FACE('',(#873),#4443,.T.);
#4679=ADVANCED_FACE('',(#874,#476),#621,.T.);
#4680=ADVANCED_FACE('',(#875),#4444,.F.);
#4681=ADVANCED_FACE('',(#876),#622,.F.);
#4682=ADVANCED_FACE('',(#877),#623,.F.);
#4683=ADVANCED_FACE('',(#878),#624,.F.);
#4684=ADVANCED_FACE('',(#879),#625,.F.);
#4685=ADVANCED_FACE('',(#880),#626,.F.);
#4686=ADVANCED_FACE('',(#881),#627,.F.);
#4687=ADVANCED_FACE('',(#882),#628,.F.);
#4688=ADVANCED_FACE('',(#883),#629,.F.);
#4689=ADVANCED_FACE('',(#884),#630,.F.);
#4690=ADVANCED_FACE('',(#885),#631,.T.);
#4691=ADVANCED_FACE('',(#886),#208,.T.);
#4692=ADVANCED_FACE('',(#887),#4445,.T.);
#4693=ADVANCED_FACE('',(#888),#209,.T.);
#4694=ADVANCED_FACE('',(#889,#477),#632,.T.);
#4695=ADVANCED_FACE('',(#890),#210,.T.);
#4696=ADVANCED_FACE('',(#891),#4446,.T.);
#4697=ADVANCED_FACE('',(#892),#4447,.F.);
#4698=ADVANCED_FACE('',(#893),#633,.T.);
#4699=ADVANCED_FACE('',(#894),#4448,.F.);
#4700=ADVANCED_FACE('',(#895),#634,.F.);
#4701=ADVANCED_FACE('',(#896),#259,.F.);
#4702=ADVANCED_FACE('',(#897),#635,.T.);
#4703=ADVANCED_FACE('',(#898,#478),#4449,.T.);
#4704=ADVANCED_FACE('',(#899),#636,.F.);
#4705=ADVANCED_FACE('',(#900,#479,#480,#481,#482),#637,.T.);
#4706=ADVANCED_FACE('',(#901),#4450,.T.);
#4707=ADVANCED_FACE('',(#902),#4451,.F.);
#4708=ADVANCED_FACE('',(#903),#4452,.F.);
#4709=ADVANCED_FACE('',(#904),#4453,.F.);
#4710=ADVANCED_FACE('',(#905),#4454,.F.);
#4711=ADVANCED_FACE('',(#906,#483,#484,#485,#486),#638,.T.);
#4712=ADVANCED_FACE('',(#907),#639,.T.);
#4713=ADVANCED_FACE('',(#908),#4455,.T.);
#4714=ADVANCED_FACE('',(#909,#487),#640,.F.);
#4715=ADVANCED_FACE('',(#910,#488),#641,.T.);
#4716=ADVANCED_FACE('',(#911),#4456,.T.);
#4717=ADVANCED_FACE('',(#912),#4457,.T.);
#4718=ADVANCED_FACE('',(#913,#489),#642,.T.);
#4719=ADVANCED_FACE('',(#914,#490),#643,.F.);
#4720=ADVANCED_FACE('',(#915),#4458,.F.);
#4721=ADVANCED_FACE('',(#916),#4459,.T.);
#4722=ADVANCED_FACE('',(#917,#491),#644,.T.);
#4723=ADVANCED_FACE('',(#918,#492),#645,.F.);
#4724=ADVANCED_FACE('',(#919),#4460,.F.);
#4725=ADVANCED_FACE('',(#920),#4461,.T.);
#4726=ADVANCED_FACE('',(#921,#493),#646,.T.);
#4727=ADVANCED_FACE('',(#922,#494),#647,.F.);
#4728=ADVANCED_FACE('',(#923),#4462,.F.);
#4729=ADVANCED_FACE('',(#924),#4463,.T.);
#4730=ADVANCED_FACE('',(#925,#495),#648,.T.);
#4731=ADVANCED_FACE('',(#926,#496),#649,.F.);
#4732=ADVANCED_FACE('',(#927),#4464,.F.);
#4733=ADVANCED_FACE('',(#928),#4465,.T.);
#4734=ADVANCED_FACE('',(#929,#497),#650,.T.);
#4735=ADVANCED_FACE('',(#930,#498),#651,.F.);
#4736=ADVANCED_FACE('',(#931),#652,.T.);
#4737=ADVANCED_FACE('',(#932),#211,.T.);
#4738=ADVANCED_FACE('',(#933),#4466,.T.);
#4739=ADVANCED_FACE('',(#934),#212,.T.);
#4740=ADVANCED_FACE('',(#935,#499),#653,.T.);
#4741=ADVANCED_FACE('',(#936),#213,.T.);
#4742=ADVANCED_FACE('',(#937),#4467,.T.);
#4743=ADVANCED_FACE('',(#938),#214,.T.);
#4744=ADVANCED_FACE('',(#939),#654,.T.);
#4745=ADVANCED_FACE('',(#940),#655,.F.);
#4746=ADVANCED_FACE('',(#941),#656,.F.);
#4747=ADVANCED_FACE('',(#942),#657,.F.);
#4748=ADVANCED_FACE('',(#943),#658,.F.);
#4749=ADVANCED_FACE('',(#944),#659,.F.);
#4750=ADVANCED_FACE('',(#945),#660,.F.);
#4751=ADVANCED_FACE('',(#946),#661,.F.);
#4752=ADVANCED_FACE('',(#947),#662,.F.);
#4753=CLOSED_SHELL('',(#4468,#4469,#4470,#4471,#4472,#4473,#4474,#4475,
#4476,#4477));
#4754=CLOSED_SHELL('',(#4478,#4479,#4480,#4481,#4482,#4483));
#4755=CLOSED_SHELL('',(#4484,#4485,#4486,#4487,#4488,#4489));
#4756=CLOSED_SHELL('',(#4490,#4491,#4492,#4493,#4494,#4495));
#4757=CLOSED_SHELL('',(#4496,#4497,#4498,#4499,#4500,#4501,#4502,#4503,
#4504,#4505));
#4758=CLOSED_SHELL('',(#4506,#4507,#4508,#4509,#4510,#4511,#4512,#4513,
#4514,#4515));
#4759=CLOSED_SHELL('',(#4516,#4517,#4518,#4519,#4520,#4521,#4522,#4523,
#4524,#4525,#4526,#4527));
#4760=CLOSED_SHELL('',(#4528,#4529,#4530,#4531,#4532,#4533,#4534,#4535,
#4536,#4537,#4538,#4539,#4540));
#4761=CLOSED_SHELL('',(#4541,#4542,#4543,#4544,#4545,#4546,#4547,#4548,
#4549,#4550,#4551,#4552));
#4762=CLOSED_SHELL('',(#4553,#4554,#4555,#4556,#4557,#4558,#4559,#4560,
#4561,#4562,#4563,#4564,#4565));
#4763=CLOSED_SHELL('',(#4566,#4567,#4568,#4569,#4570,#4571,#4572,#4573,
#4574,#4575,#4576,#4577,#4578));
#4764=CLOSED_SHELL('',(#4579));
#4765=CLOSED_SHELL('',(#4580,#4581,#4582,#4583,#4584));
#4766=CLOSED_SHELL('',(#4585,#4586,#4587,#4588,#4589,#4590));
#4767=CLOSED_SHELL('',(#4591,#4592,#4593,#4594));
#4768=CLOSED_SHELL('',(#4595,#4596,#4597));
#4769=CLOSED_SHELL('',(#4598,#4599,#4600,#4601,#4602,#4603));
#4770=CLOSED_SHELL('',(#4604,#4605,#4606,#4607,#4608,#4609));
#4771=CLOSED_SHELL('',(#4610,#4611,#4612,#4613));
#4772=CLOSED_SHELL('',(#4614,#4615,#4616,#4617,#4618,#4619,#4620,#4621));
#4773=CLOSED_SHELL('',(#4622,#4623,#4624,#4625,#4626,#4627,#4628,#4629));
#4774=CLOSED_SHELL('',(#4630,#4631,#4632,#4633,#4634,#4635,#4636,#4637));
#4775=CLOSED_SHELL('',(#4638,#4639,#4640,#4641,#4642,#4643,#4644,#4645));
#4776=CLOSED_SHELL('',(#4646));
#4777=CLOSED_SHELL('',(#4647));
#4778=CLOSED_SHELL('',(#4648));
#4779=CLOSED_SHELL('',(#4649));
#4780=CLOSED_SHELL('',(#4650));
#4781=CLOSED_SHELL('',(#4651));
#4782=CLOSED_SHELL('',(#4652));
#4783=CLOSED_SHELL('',(#4653));
#4784=CLOSED_SHELL('',(#4654,#4655,#4656,#4657,#4658,#4659,#4660,#4661,
#4662,#4663,#4664,#4665,#4666,#4667,#4668,#4669,#4670,#4671,#4672));
#4785=CLOSED_SHELL('',(#4673,#4674,#4675,#4676));
#4786=CLOSED_SHELL('',(#4677,#4678,#4679,#4680));
#4787=CLOSED_SHELL('',(#4681,#4682,#4683,#4684,#4685,#4686,#4687,#4688));
#4788=CLOSED_SHELL('',(#4689,#4690,#4691,#4692,#4693,#4694,#4695,#4696));
#4789=CLOSED_SHELL('',(#4697,#4698,#4699,#4700,#4701,#4702,#4703,#4704,
#4705,#4706,#4707,#4708,#4709,#4710,#4711,#4712,#4713,#4714,#4715,#4716,
#4717,#4718,#4719));
#4790=CLOSED_SHELL('',(#4720,#4721,#4722,#4723));
#4791=CLOSED_SHELL('',(#4724,#4725,#4726,#4727));
#4792=CLOSED_SHELL('',(#4728,#4729,#4730,#4731));
#4793=CLOSED_SHELL('',(#4732,#4733,#4734,#4735));
#4794=CLOSED_SHELL('',(#4736,#4737,#4738,#4739,#4740,#4741,#4742,#4743,
#4744));
#4795=CLOSED_SHELL('',(#4745,#4746,#4747,#4748,#4749,#4750,#4751,#4752));
#4796=DERIVED_UNIT_ELEMENT(#4858,1.);
#4797=DERIVED_UNIT_ELEMENT(#9815,-3.);
#4798=DERIVED_UNIT_ELEMENT(#4858,1.);
#4799=DERIVED_UNIT_ELEMENT(#9815,-3.);
#4800=DERIVED_UNIT_ELEMENT(#4858,1.);
#4801=DERIVED_UNIT_ELEMENT(#9815,-3.);
#4802=DERIVED_UNIT_ELEMENT(#4858,1.);
#4803=DERIVED_UNIT_ELEMENT(#9815,-3.);
#4804=DERIVED_UNIT_ELEMENT(#4858,1.);
#4805=DERIVED_UNIT_ELEMENT(#9815,-3.);
#4806=DERIVED_UNIT_ELEMENT(#4858,1.);
#4807=DERIVED_UNIT_ELEMENT(#9815,-3.);
#4808=DERIVED_UNIT_ELEMENT(#4858,1.);
#4809=DERIVED_UNIT_ELEMENT(#9815,-3.);
#4810=DERIVED_UNIT_ELEMENT(#4858,1.);
#4811=DERIVED_UNIT_ELEMENT(#9815,-3.);
#4812=DERIVED_UNIT_ELEMENT(#4858,1.);
#4813=DERIVED_UNIT_ELEMENT(#9815,-3.);
#4814=DERIVED_UNIT_ELEMENT(#4858,1.);
#4815=DERIVED_UNIT_ELEMENT(#9815,-3.);
#4816=DERIVED_UNIT_ELEMENT(#4858,1.);
#4817=DERIVED_UNIT_ELEMENT(#9815,-3.);
#4818=DERIVED_UNIT_ELEMENT(#4858,1.);
#4819=DERIVED_UNIT_ELEMENT(#9815,-3.);
#4820=DERIVED_UNIT_ELEMENT(#4858,1.);
#4821=DERIVED_UNIT_ELEMENT(#9815,-3.);
#4822=DERIVED_UNIT_ELEMENT(#4858,1.);
#4823=DERIVED_UNIT_ELEMENT(#9815,-3.);
#4824=DERIVED_UNIT_ELEMENT(#4858,1.);
#4825=DERIVED_UNIT_ELEMENT(#9815,-3.);
#4826=DERIVED_UNIT_ELEMENT(#4858,1.);
#4827=DERIVED_UNIT_ELEMENT(#9815,-3.);
#4828=DERIVED_UNIT_ELEMENT(#4858,1.);
#4829=DERIVED_UNIT_ELEMENT(#9815,-3.);
#4830=DERIVED_UNIT_ELEMENT(#4858,1.);
#4831=DERIVED_UNIT_ELEMENT(#9815,-3.);
#4832=DERIVED_UNIT_ELEMENT(#4858,1.);
#4833=DERIVED_UNIT_ELEMENT(#9815,-3.);
#4834=DERIVED_UNIT_ELEMENT(#4858,1.);
#4835=DERIVED_UNIT_ELEMENT(#9815,-3.);
#4836=DERIVED_UNIT_ELEMENT(#4858,1.);
#4837=DERIVED_UNIT_ELEMENT(#9815,-3.);
#4838=DERIVED_UNIT_ELEMENT(#4858,1.);
#4839=DERIVED_UNIT_ELEMENT(#9815,-3.);
#4840=DERIVED_UNIT_ELEMENT(#4858,1.);
#4841=DERIVED_UNIT_ELEMENT(#9815,-3.);
#4842=DERIVED_UNIT_ELEMENT(#4858,1.);
#4843=DERIVED_UNIT_ELEMENT(#9815,-3.);
#4844=DERIVED_UNIT_ELEMENT(#4858,1.);
#4845=DERIVED_UNIT_ELEMENT(#9815,-3.);
#4846=DERIVED_UNIT_ELEMENT(#4858,1.);
#4847=DERIVED_UNIT_ELEMENT(#9815,-3.);
#4848=DERIVED_UNIT_ELEMENT(#4858,1.);
#4849=DERIVED_UNIT_ELEMENT(#9815,-3.);
#4850=DERIVED_UNIT_ELEMENT(#4858,1.);
#4851=DERIVED_UNIT_ELEMENT(#9815,-3.);
#4852=DERIVED_UNIT_ELEMENT(#4858,1.);
#4853=DERIVED_UNIT_ELEMENT(#9815,-3.);
#4854=DERIVED_UNIT_ELEMENT(#4858,1.);
#4855=DERIVED_UNIT_ELEMENT(#9815,-3.);
#4856=DERIVED_UNIT_ELEMENT(#4858,1.);
#4857=DERIVED_UNIT_ELEMENT(#9815,-3.);
#4858=(
MASS_UNIT()
NAMED_UNIT(*)
SI_UNIT(.KILO.,.GRAM.)
);
#4859=DERIVED_UNIT((#4796,#4797));
#4860=DERIVED_UNIT((#4798,#4799));
#4861=DERIVED_UNIT((#4800,#4801));
#4862=DERIVED_UNIT((#4802,#4803));
#4863=DERIVED_UNIT((#4804,#4805));
#4864=DERIVED_UNIT((#4806,#4807));
#4865=DERIVED_UNIT((#4808,#4809));
#4866=DERIVED_UNIT((#4810,#4811));
#4867=DERIVED_UNIT((#4812,#4813));
#4868=DERIVED_UNIT((#4814,#4815));
#4869=DERIVED_UNIT((#4816,#4817));
#4870=DERIVED_UNIT((#4818,#4819));
#4871=DERIVED_UNIT((#4820,#4821));
#4872=DERIVED_UNIT((#4822,#4823));
#4873=DERIVED_UNIT((#4824,#4825));
#4874=DERIVED_UNIT((#4826,#4827));
#4875=DERIVED_UNIT((#4828,#4829));
#4876=DERIVED_UNIT((#4830,#4831));
#4877=DERIVED_UNIT((#4832,#4833));
#4878=DERIVED_UNIT((#4834,#4835));
#4879=DERIVED_UNIT((#4836,#4837));
#4880=DERIVED_UNIT((#4838,#4839));
#4881=DERIVED_UNIT((#4840,#4841));
#4882=DERIVED_UNIT((#4842,#4843));
#4883=DERIVED_UNIT((#4844,#4845));
#4884=DERIVED_UNIT((#4846,#4847));
#4885=DERIVED_UNIT((#4848,#4849));
#4886=DERIVED_UNIT((#4850,#4851));
#4887=DERIVED_UNIT((#4852,#4853));
#4888=DERIVED_UNIT((#4854,#4855));
#4889=DERIVED_UNIT((#4856,#4857));
#4890=MEASURE_REPRESENTATION_ITEM('density measure',
POSITIVE_RATIO_MEASURE(7850.),#4859);
#4891=MEASURE_REPRESENTATION_ITEM('density measure',
POSITIVE_RATIO_MEASURE(7850.),#4860);
#4892=MEASURE_REPRESENTATION_ITEM('density measure',
POSITIVE_RATIO_MEASURE(7850.),#4861);
#4893=MEASURE_REPRESENTATION_ITEM('density measure',
POSITIVE_RATIO_MEASURE(7850.),#4862);
#4894=MEASURE_REPRESENTATION_ITEM('density measure',
POSITIVE_RATIO_MEASURE(7850.),#4863);
#4895=MEASURE_REPRESENTATION_ITEM('density measure',
POSITIVE_RATIO_MEASURE(7850.),#4864);
#4896=MEASURE_REPRESENTATION_ITEM('density measure',
POSITIVE_RATIO_MEASURE(7850.),#4865);
#4897=MEASURE_REPRESENTATION_ITEM('density measure',
POSITIVE_RATIO_MEASURE(7850.),#4866);
#4898=MEASURE_REPRESENTATION_ITEM('density measure',
POSITIVE_RATIO_MEASURE(7850.),#4867);
#4899=MEASURE_REPRESENTATION_ITEM('density measure',
POSITIVE_RATIO_MEASURE(7850.),#4868);
#4900=MEASURE_REPRESENTATION_ITEM('density measure',
POSITIVE_RATIO_MEASURE(7850.),#4869);
#4901=MEASURE_REPRESENTATION_ITEM('density measure',
POSITIVE_RATIO_MEASURE(7850.),#4870);
#4902=MEASURE_REPRESENTATION_ITEM('density measure',
POSITIVE_RATIO_MEASURE(7850.),#4871);
#4903=MEASURE_REPRESENTATION_ITEM('density measure',
POSITIVE_RATIO_MEASURE(7850.),#4872);
#4904=MEASURE_REPRESENTATION_ITEM('density measure',
POSITIVE_RATIO_MEASURE(7850.),#4873);
#4905=MEASURE_REPRESENTATION_ITEM('density measure',
POSITIVE_RATIO_MEASURE(7850.),#4874);
#4906=MEASURE_REPRESENTATION_ITEM('density measure',
POSITIVE_RATIO_MEASURE(7850.),#4875);
#4907=MEASURE_REPRESENTATION_ITEM('density measure',
POSITIVE_RATIO_MEASURE(7850.),#4876);
#4908=MEASURE_REPRESENTATION_ITEM('density measure',
POSITIVE_RATIO_MEASURE(7850.),#4877);
#4909=MEASURE_REPRESENTATION_ITEM('density measure',
POSITIVE_RATIO_MEASURE(7850.),#4878);
#4910=MEASURE_REPRESENTATION_ITEM('density measure',
POSITIVE_RATIO_MEASURE(7850.),#4879);
#4911=MEASURE_REPRESENTATION_ITEM('density measure',
POSITIVE_RATIO_MEASURE(7850.),#4880);
#4912=MEASURE_REPRESENTATION_ITEM('density measure',
POSITIVE_RATIO_MEASURE(7850.),#4881);
#4913=MEASURE_REPRESENTATION_ITEM('density measure',
POSITIVE_RATIO_MEASURE(7850.),#4882);
#4914=MEASURE_REPRESENTATION_ITEM('density measure',
POSITIVE_RATIO_MEASURE(7850.),#4883);
#4915=MEASURE_REPRESENTATION_ITEM('density measure',
POSITIVE_RATIO_MEASURE(7850.),#4884);
#4916=MEASURE_REPRESENTATION_ITEM('density measure',
POSITIVE_RATIO_MEASURE(7850.),#4885);
#4917=MEASURE_REPRESENTATION_ITEM('density measure',
POSITIVE_RATIO_MEASURE(7850.),#4886);
#4918=MEASURE_REPRESENTATION_ITEM('density measure',
POSITIVE_RATIO_MEASURE(7850.),#4887);
#4919=MEASURE_REPRESENTATION_ITEM('density measure',
POSITIVE_RATIO_MEASURE(7850.),#4888);
#4920=MEASURE_REPRESENTATION_ITEM('density measure',
POSITIVE_RATIO_MEASURE(7850.),#4889);
#4921=PROPERTY_DEFINITION_REPRESENTATION(#5076,#4983);
#4922=PROPERTY_DEFINITION_REPRESENTATION(#5077,#4984);
#4923=PROPERTY_DEFINITION_REPRESENTATION(#5078,#4985);
#4924=PROPERTY_DEFINITION_REPRESENTATION(#5079,#4986);
#4925=PROPERTY_DEFINITION_REPRESENTATION(#5080,#4987);
#4926=PROPERTY_DEFINITION_REPRESENTATION(#5081,#4988);
#4927=PROPERTY_DEFINITION_REPRESENTATION(#5082,#4989);
#4928=PROPERTY_DEFINITION_REPRESENTATION(#5083,#4990);
#4929=PROPERTY_DEFINITION_REPRESENTATION(#5084,#4991);
#4930=PROPERTY_DEFINITION_REPRESENTATION(#5085,#4992);
#4931=PROPERTY_DEFINITION_REPRESENTATION(#5086,#4993);
#4932=PROPERTY_DEFINITION_REPRESENTATION(#5087,#4994);
#4933=PROPERTY_DEFINITION_REPRESENTATION(#5088,#4995);
#4934=PROPERTY_DEFINITION_REPRESENTATION(#5089,#4996);
#4935=PROPERTY_DEFINITION_REPRESENTATION(#5090,#4997);
#4936=PROPERTY_DEFINITION_REPRESENTATION(#5091,#4998);
#4937=PROPERTY_DEFINITION_REPRESENTATION(#5092,#4999);
#4938=PROPERTY_DEFINITION_REPRESENTATION(#5093,#5000);
#4939=PROPERTY_DEFINITION_REPRESENTATION(#5094,#5001);
#4940=PROPERTY_DEFINITION_REPRESENTATION(#5095,#5002);
#4941=PROPERTY_DEFINITION_REPRESENTATION(#5096,#5003);
#4942=PROPERTY_DEFINITION_REPRESENTATION(#5097,#5004);
#4943=PROPERTY_DEFINITION_REPRESENTATION(#5098,#5005);
#4944=PROPERTY_DEFINITION_REPRESENTATION(#5099,#5006);
#4945=PROPERTY_DEFINITION_REPRESENTATION(#5100,#5007);
#4946=PROPERTY_DEFINITION_REPRESENTATION(#5101,#5008);
#4947=PROPERTY_DEFINITION_REPRESENTATION(#5102,#5009);
#4948=PROPERTY_DEFINITION_REPRESENTATION(#5103,#5010);
#4949=PROPERTY_DEFINITION_REPRESENTATION(#5104,#5011);
#4950=PROPERTY_DEFINITION_REPRESENTATION(#5105,#5012);
#4951=PROPERTY_DEFINITION_REPRESENTATION(#5106,#5013);
#4952=PROPERTY_DEFINITION_REPRESENTATION(#5107,#5014);
#4953=PROPERTY_DEFINITION_REPRESENTATION(#5108,#5015);
#4954=PROPERTY_DEFINITION_REPRESENTATION(#5109,#5016);
#4955=PROPERTY_DEFINITION_REPRESENTATION(#5110,#5017);
#4956=PROPERTY_DEFINITION_REPRESENTATION(#5111,#5018);
#4957=PROPERTY_DEFINITION_REPRESENTATION(#5112,#5019);
#4958=PROPERTY_DEFINITION_REPRESENTATION(#5113,#5020);
#4959=PROPERTY_DEFINITION_REPRESENTATION(#5114,#5021);
#4960=PROPERTY_DEFINITION_REPRESENTATION(#5115,#5022);
#4961=PROPERTY_DEFINITION_REPRESENTATION(#5116,#5023);
#4962=PROPERTY_DEFINITION_REPRESENTATION(#5117,#5024);
#4963=PROPERTY_DEFINITION_REPRESENTATION(#5118,#5025);
#4964=PROPERTY_DEFINITION_REPRESENTATION(#5119,#5026);
#4965=PROPERTY_DEFINITION_REPRESENTATION(#5120,#5027);
#4966=PROPERTY_DEFINITION_REPRESENTATION(#5121,#5028);
#4967=PROPERTY_DEFINITION_REPRESENTATION(#5122,#5029);
#4968=PROPERTY_DEFINITION_REPRESENTATION(#5123,#5030);
#4969=PROPERTY_DEFINITION_REPRESENTATION(#5124,#5031);
#4970=PROPERTY_DEFINITION_REPRESENTATION(#5125,#5032);
#4971=PROPERTY_DEFINITION_REPRESENTATION(#5126,#5033);
#4972=PROPERTY_DEFINITION_REPRESENTATION(#5127,#5034);
#4973=PROPERTY_DEFINITION_REPRESENTATION(#5128,#5035);
#4974=PROPERTY_DEFINITION_REPRESENTATION(#5129,#5036);
#4975=PROPERTY_DEFINITION_REPRESENTATION(#5130,#5037);
#4976=PROPERTY_DEFINITION_REPRESENTATION(#5131,#5038);
#4977=PROPERTY_DEFINITION_REPRESENTATION(#5132,#5039);
#4978=PROPERTY_DEFINITION_REPRESENTATION(#5133,#5040);
#4979=PROPERTY_DEFINITION_REPRESENTATION(#5134,#5041);
#4980=PROPERTY_DEFINITION_REPRESENTATION(#5135,#5042);
#4981=PROPERTY_DEFINITION_REPRESENTATION(#5136,#5043);
#4982=PROPERTY_DEFINITION_REPRESENTATION(#5137,#5044);
#4983=REPRESENTATION('material name',(#5045),#9780);
#4984=REPRESENTATION('density',(#4890),#9780);
#4985=REPRESENTATION('material name',(#5046),#9781);
#4986=REPRESENTATION('density',(#4891),#9781);
#4987=REPRESENTATION('material name',(#5047),#9782);
#4988=REPRESENTATION('density',(#4892),#9782);
#4989=REPRESENTATION('material name',(#5048),#9783);
#4990=REPRESENTATION('density',(#4893),#9783);
#4991=REPRESENTATION('material name',(#5049),#9784);
#4992=REPRESENTATION('density',(#4894),#9784);
#4993=REPRESENTATION('material name',(#5050),#9785);
#4994=REPRESENTATION('density',(#4895),#9785);
#4995=REPRESENTATION('material name',(#5051),#9786);
#4996=REPRESENTATION('density',(#4896),#9786);
#4997=REPRESENTATION('material name',(#5052),#9787);
#4998=REPRESENTATION('density',(#4897),#9787);
#4999=REPRESENTATION('material name',(#5053),#9788);
#5000=REPRESENTATION('density',(#4898),#9788);
#5001=REPRESENTATION('material name',(#5054),#9789);
#5002=REPRESENTATION('density',(#4899),#9789);
#5003=REPRESENTATION('material name',(#5055),#9790);
#5004=REPRESENTATION('density',(#4900),#9790);
#5005=REPRESENTATION('material name',(#5056),#9791);
#5006=REPRESENTATION('density',(#4901),#9791);
#5007=REPRESENTATION('material name',(#5057),#9792);
#5008=REPRESENTATION('density',(#4902),#9792);
#5009=REPRESENTATION('material name',(#5058),#9793);
#5010=REPRESENTATION('density',(#4903),#9793);
#5011=REPRESENTATION('material name',(#5059),#9794);
#5012=REPRESENTATION('density',(#4904),#9794);
#5013=REPRESENTATION('material name',(#5060),#9795);
#5014=REPRESENTATION('density',(#4905),#9795);
#5015=REPRESENTATION('material name',(#5061),#9796);
#5016=REPRESENTATION('density',(#4906),#9796);
#5017=REPRESENTATION('material name',(#5062),#9797);
#5018=REPRESENTATION('density',(#4907),#9797);
#5019=REPRESENTATION('material name',(#5063),#9798);
#5020=REPRESENTATION('density',(#4908),#9798);
#5021=REPRESENTATION('material name',(#5064),#9800);
#5022=REPRESENTATION('density',(#4909),#9800);
#5023=REPRESENTATION('material name',(#5065),#9801);
#5024=REPRESENTATION('density',(#4910),#9801);
#5025=REPRESENTATION('material name',(#5066),#9802);
#5026=REPRESENTATION('density',(#4911),#9802);
#5027=REPRESENTATION('material name',(#5067),#9803);
#5028=REPRESENTATION('density',(#4912),#9803);
#5029=REPRESENTATION('material name',(#5068),#9804);
#5030=REPRESENTATION('density',(#4913),#9804);
#5031=REPRESENTATION('material name',(#5069),#9805);
#5032=REPRESENTATION('density',(#4914),#9805);
#5033=REPRESENTATION('material name',(#5070),#9807);
#5034=REPRESENTATION('density',(#4915),#9807);
#5035=REPRESENTATION('material name',(#5071),#9808);
#5036=REPRESENTATION('density',(#4916),#9808);
#5037=REPRESENTATION('material name',(#5072),#9809);
#5038=REPRESENTATION('density',(#4917),#9809);
#5039=REPRESENTATION('material name',(#5073),#9810);
#5040=REPRESENTATION('density',(#4918),#9810);
#5041=REPRESENTATION('material name',(#5074),#9811);
#5042=REPRESENTATION('density',(#4919),#9811);
#5043=REPRESENTATION('material name',(#5075),#9812);
#5044=REPRESENTATION('density',(#4920),#9812);
#5045=DESCRIPTIVE_REPRESENTATION_ITEM('Steel','Steel');
#5046=DESCRIPTIVE_REPRESENTATION_ITEM('Steel','Steel');
#5047=DESCRIPTIVE_REPRESENTATION_ITEM('Steel','Steel');
#5048=DESCRIPTIVE_REPRESENTATION_ITEM('Steel','Steel');
#5049=DESCRIPTIVE_REPRESENTATION_ITEM('Steel','Steel');
#5050=DESCRIPTIVE_REPRESENTATION_ITEM('Steel','Steel');
#5051=DESCRIPTIVE_REPRESENTATION_ITEM('Steel','Steel');
#5052=DESCRIPTIVE_REPRESENTATION_ITEM('Steel','Steel');
#5053=DESCRIPTIVE_REPRESENTATION_ITEM('Steel','Steel');
#5054=DESCRIPTIVE_REPRESENTATION_ITEM('Steel','Steel');
#5055=DESCRIPTIVE_REPRESENTATION_ITEM('Steel','Steel');
#5056=DESCRIPTIVE_REPRESENTATION_ITEM('Steel','Steel');
#5057=DESCRIPTIVE_REPRESENTATION_ITEM('Steel','Steel');
#5058=DESCRIPTIVE_REPRESENTATION_ITEM('Steel','Steel');
#5059=DESCRIPTIVE_REPRESENTATION_ITEM('Steel','Steel');
#5060=DESCRIPTIVE_REPRESENTATION_ITEM('Steel','Steel');
#5061=DESCRIPTIVE_REPRESENTATION_ITEM('Steel','Steel');
#5062=DESCRIPTIVE_REPRESENTATION_ITEM('Steel','Steel');
#5063=DESCRIPTIVE_REPRESENTATION_ITEM('Steel','Steel');
#5064=DESCRIPTIVE_REPRESENTATION_ITEM('Steel','Steel');
#5065=DESCRIPTIVE_REPRESENTATION_ITEM('Steel','Steel');
#5066=DESCRIPTIVE_REPRESENTATION_ITEM('Steel','Steel');
#5067=DESCRIPTIVE_REPRESENTATION_ITEM('Steel','Steel');
#5068=DESCRIPTIVE_REPRESENTATION_ITEM('Steel','Steel');
#5069=DESCRIPTIVE_REPRESENTATION_ITEM('Steel','Steel');
#5070=DESCRIPTIVE_REPRESENTATION_ITEM('Steel','Steel');
#5071=DESCRIPTIVE_REPRESENTATION_ITEM('Steel','Steel');
#5072=DESCRIPTIVE_REPRESENTATION_ITEM('Steel','Steel');
#5073=DESCRIPTIVE_REPRESENTATION_ITEM('Steel','Steel');
#5074=DESCRIPTIVE_REPRESENTATION_ITEM('Steel','Steel');
#5075=DESCRIPTIVE_REPRESENTATION_ITEM('Steel','Steel');
#5076=PROPERTY_DEFINITION('material property','material name',#9973);
#5077=PROPERTY_DEFINITION('material property','density of part',#9973);
#5078=PROPERTY_DEFINITION('material property','material name',#9974);
#5079=PROPERTY_DEFINITION('material property','density of part',#9974);
#5080=PROPERTY_DEFINITION('material property','material name',#9975);
#5081=PROPERTY_DEFINITION('material property','density of part',#9975);
#5082=PROPERTY_DEFINITION('material property','material name',#9976);
#5083=PROPERTY_DEFINITION('material property','density of part',#9976);
#5084=PROPERTY_DEFINITION('material property','material name',#9977);
#5085=PROPERTY_DEFINITION('material property','density of part',#9977);
#5086=PROPERTY_DEFINITION('material property','material name',#9978);
#5087=PROPERTY_DEFINITION('material property','density of part',#9978);
#5088=PROPERTY_DEFINITION('material property','material name',#9979);
#5089=PROPERTY_DEFINITION('material property','density of part',#9979);
#5090=PROPERTY_DEFINITION('material property','material name',#9980);
#5091=PROPERTY_DEFINITION('material property','density of part',#9980);
#5092=PROPERTY_DEFINITION('material property','material name',#9981);
#5093=PROPERTY_DEFINITION('material property','density of part',#9981);
#5094=PROPERTY_DEFINITION('material property','material name',#9982);
#5095=PROPERTY_DEFINITION('material property','density of part',#9982);
#5096=PROPERTY_DEFINITION('material property','material name',#9983);
#5097=PROPERTY_DEFINITION('material property','density of part',#9983);
#5098=PROPERTY_DEFINITION('material property','material name',#9984);
#5099=PROPERTY_DEFINITION('material property','density of part',#9984);
#5100=PROPERTY_DEFINITION('material property','material name',#9985);
#5101=PROPERTY_DEFINITION('material property','density of part',#9985);
#5102=PROPERTY_DEFINITION('material property','material name',#9986);
#5103=PROPERTY_DEFINITION('material property','density of part',#9986);
#5104=PROPERTY_DEFINITION('material property','material name',#9987);
#5105=PROPERTY_DEFINITION('material property','density of part',#9987);
#5106=PROPERTY_DEFINITION('material property','material name',#9988);
#5107=PROPERTY_DEFINITION('material property','density of part',#9988);
#5108=PROPERTY_DEFINITION('material property','material name',#9989);
#5109=PROPERTY_DEFINITION('material property','density of part',#9989);
#5110=PROPERTY_DEFINITION('material property','material name',#9990);
#5111=PROPERTY_DEFINITION('material property','density of part',#9990);
#5112=PROPERTY_DEFINITION('material property','material name',#9991);
#5113=PROPERTY_DEFINITION('material property','density of part',#9991);
#5114=PROPERTY_DEFINITION('material property','material name',#9993);
#5115=PROPERTY_DEFINITION('material property','density of part',#9993);
#5116=PROPERTY_DEFINITION('material property','material name',#9994);
#5117=PROPERTY_DEFINITION('material property','density of part',#9994);
#5118=PROPERTY_DEFINITION('material property','material name',#9995);
#5119=PROPERTY_DEFINITION('material property','density of part',#9995);
#5120=PROPERTY_DEFINITION('material property','material name',#9996);
#5121=PROPERTY_DEFINITION('material property','density of part',#9996);
#5122=PROPERTY_DEFINITION('material property','material name',#9997);
#5123=PROPERTY_DEFINITION('material property','density of part',#9997);
#5124=PROPERTY_DEFINITION('material property','material name',#9998);
#5125=PROPERTY_DEFINITION('material property','density of part',#9998);
#5126=PROPERTY_DEFINITION('material property','material name',#10000);
#5127=PROPERTY_DEFINITION('material property','density of part',#10000);
#5128=PROPERTY_DEFINITION('material property','material name',#10001);
#5129=PROPERTY_DEFINITION('material property','density of part',#10001);
#5130=PROPERTY_DEFINITION('material property','material name',#10002);
#5131=PROPERTY_DEFINITION('material property','density of part',#10002);
#5132=PROPERTY_DEFINITION('material property','material name',#10003);
#5133=PROPERTY_DEFINITION('material property','density of part',#10003);
#5134=PROPERTY_DEFINITION('material property','material name',#10004);
#5135=PROPERTY_DEFINITION('material property','density of part',#10004);
#5136=PROPERTY_DEFINITION('material property','material name',#10005);
#5137=PROPERTY_DEFINITION('material property','density of part',#10005);
#5138=AXIS2_PLACEMENT_3D('',#7297,#5751,#5752);
#5139=AXIS2_PLACEMENT_3D('',#7298,#5753,#5754);
#5140=AXIS2_PLACEMENT_3D('',#7299,#5755,#5756);
#5141=AXIS2_PLACEMENT_3D('',#7300,#5757,#5758);
#5142=AXIS2_PLACEMENT_3D('',#7302,#5759,#5760);
#5143=AXIS2_PLACEMENT_3D('',#7305,#5762,#5763);
#5144=AXIS2_PLACEMENT_3D('',#7306,#5764,#5765);
#5145=AXIS2_PLACEMENT_3D('',#7308,#5766,#5767);
#5146=AXIS2_PLACEMENT_3D('',#7311,#5769,#5770);
#5147=AXIS2_PLACEMENT_3D('',#7312,#5771,#5772);
#5148=AXIS2_PLACEMENT_3D('',#7314,#5773,#5774);
#5149=AXIS2_PLACEMENT_3D('',#7317,#5776,#5777);
#5150=AXIS2_PLACEMENT_3D('',#7318,#5778,#5779);
#5151=AXIS2_PLACEMENT_3D('',#7320,#5780,#5781);
#5152=AXIS2_PLACEMENT_3D('',#7323,#5783,#5784);
#5153=AXIS2_PLACEMENT_3D('',#7324,#5785,#5786);
#5154=AXIS2_PLACEMENT_3D('',#7333,#5791,#5792);
#5155=AXIS2_PLACEMENT_3D('',#7339,#5796,#5797);
#5156=AXIS2_PLACEMENT_3D('',#7345,#5801,#5802);
#5157=AXIS2_PLACEMENT_3D('',#7348,#5805,#5806);
#5158=AXIS2_PLACEMENT_3D('',#7349,#5807,#5808);
#5159=AXIS2_PLACEMENT_3D('',#7350,#5809,#5810);
#5160=AXIS2_PLACEMENT_3D('',#7351,#5811,#5812);
#5161=AXIS2_PLACEMENT_3D('',#7360,#5817,#5818);
#5162=AXIS2_PLACEMENT_3D('',#7366,#5822,#5823);
#5163=AXIS2_PLACEMENT_3D('',#7372,#5827,#5828);
#5164=AXIS2_PLACEMENT_3D('',#7375,#5831,#5832);
#5165=AXIS2_PLACEMENT_3D('',#7376,#5833,#5834);
#5166=AXIS2_PLACEMENT_3D('',#7377,#5835,#5836);
#5167=AXIS2_PLACEMENT_3D('',#7378,#5837,#5838);
#5168=AXIS2_PLACEMENT_3D('',#7387,#5843,#5844);
#5169=AXIS2_PLACEMENT_3D('',#7393,#5848,#5849);
#5170=AXIS2_PLACEMENT_3D('',#7399,#5853,#5854);
#5171=AXIS2_PLACEMENT_3D('',#7402,#5857,#5858);
#5172=AXIS2_PLACEMENT_3D('',#7403,#5859,#5860);
#5173=AXIS2_PLACEMENT_3D('',#7404,#5861,#5862);
#5174=AXIS2_PLACEMENT_3D('',#7405,#5863,#5864);
#5175=AXIS2_PLACEMENT_3D('',#7414,#5869,#5870);
#5176=AXIS2_PLACEMENT_3D('',#7420,#5874,#5875);
#5177=AXIS2_PLACEMENT_3D('',#7426,#5879,#5880);
#5178=AXIS2_PLACEMENT_3D('',#7429,#5883,#5884);
#5179=AXIS2_PLACEMENT_3D('',#7430,#5885,#5886);
#5180=AXIS2_PLACEMENT_3D('',#7431,#5887,#5888);
#5181=AXIS2_PLACEMENT_3D('',#7433,#5889,#5890);
#5182=AXIS2_PLACEMENT_3D('',#7436,#5892,#5893);
#5183=AXIS2_PLACEMENT_3D('',#7437,#5894,#5895);
#5184=AXIS2_PLACEMENT_3D('',#7439,#5896,#5897);
#5185=AXIS2_PLACEMENT_3D('',#7442,#5899,#5900);
#5186=AXIS2_PLACEMENT_3D('',#7443,#5901,#5902);
#5187=AXIS2_PLACEMENT_3D('',#7445,#5903,#5904);
#5188=AXIS2_PLACEMENT_3D('',#7448,#5906,#5907);
#5189=AXIS2_PLACEMENT_3D('',#7449,#5908,#5909);
#5190=AXIS2_PLACEMENT_3D('',#7451,#5910,#5911);
#5191=AXIS2_PLACEMENT_3D('',#7454,#5913,#5914);
#5192=AXIS2_PLACEMENT_3D('',#7455,#5915,#5916);
#5193=AXIS2_PLACEMENT_3D('',#7464,#5921,#5922);
#5194=AXIS2_PLACEMENT_3D('',#7470,#5926,#5927);
#5195=AXIS2_PLACEMENT_3D('',#7476,#5931,#5932);
#5196=AXIS2_PLACEMENT_3D('',#7479,#5935,#5936);
#5197=AXIS2_PLACEMENT_3D('',#7480,#5937,#5938);
#5198=AXIS2_PLACEMENT_3D('',#7481,#5939,#5940);
#5199=AXIS2_PLACEMENT_3D('',#7482,#5941,#5942);
#5200=AXIS2_PLACEMENT_3D('',#7484,#5943,#5944);
#5201=AXIS2_PLACEMENT_3D('',#7487,#5946,#5947);
#5202=AXIS2_PLACEMENT_3D('',#7488,#5948,#5949);
#5203=AXIS2_PLACEMENT_3D('',#7490,#5950,#5951);
#5204=AXIS2_PLACEMENT_3D('',#7493,#5953,#5954);
#5205=AXIS2_PLACEMENT_3D('',#7494,#5955,#5956);
#5206=AXIS2_PLACEMENT_3D('',#7496,#5957,#5958);
#5207=AXIS2_PLACEMENT_3D('',#7499,#5960,#5961);
#5208=AXIS2_PLACEMENT_3D('',#7500,#5962,#5963);
#5209=AXIS2_PLACEMENT_3D('',#7502,#5964,#5965);
#5210=AXIS2_PLACEMENT_3D('',#7505,#5967,#5968);
#5211=AXIS2_PLACEMENT_3D('',#7506,#5969,#5970);
#5212=AXIS2_PLACEMENT_3D('',#7515,#5975,#5976);
#5213=AXIS2_PLACEMENT_3D('',#7521,#5980,#5981);
#5214=AXIS2_PLACEMENT_3D('',#7527,#5985,#5986);
#5215=AXIS2_PLACEMENT_3D('',#7530,#5989,#5990);
#5216=AXIS2_PLACEMENT_3D('',#7531,#5991,#5992);
#5217=AXIS2_PLACEMENT_3D('',#7532,#5993,#5994);
#5218=AXIS2_PLACEMENT_3D('',#7533,#5995,#5996);
#5219=AXIS2_PLACEMENT_3D('',#7535,#5997,#5998);
#5220=AXIS2_PLACEMENT_3D('',#7538,#6000,#6001);
#5221=AXIS2_PLACEMENT_3D('',#7539,#6002,#6003);
#5222=AXIS2_PLACEMENT_3D('',#7541,#6004,#6005);
#5223=AXIS2_PLACEMENT_3D('',#7544,#6007,#6008);
#5224=AXIS2_PLACEMENT_3D('',#7545,#6009,#6010);
#5225=AXIS2_PLACEMENT_3D('',#7547,#6011,#6012);
#5226=AXIS2_PLACEMENT_3D('',#7550,#6014,#6015);
#5227=AXIS2_PLACEMENT_3D('',#7551,#6016,#6017);
#5228=AXIS2_PLACEMENT_3D('',#7553,#6018,#6019);
#5229=AXIS2_PLACEMENT_3D('',#7556,#6021,#6022);
#5230=AXIS2_PLACEMENT_3D('',#7557,#6023,#6024);
#5231=AXIS2_PLACEMENT_3D('',#7559,#6025,#6026);
#5232=AXIS2_PLACEMENT_3D('',#7560,#6027,#6028);
#5233=AXIS2_PLACEMENT_3D('',#7562,#6029,#6030);
#5234=AXIS2_PLACEMENT_3D('',#7564,#6032,#6033);
#5235=AXIS2_PLACEMENT_3D('',#7572,#6037,#6038);
#5236=AXIS2_PLACEMENT_3D('',#7573,#6039,#6040);
#5237=AXIS2_PLACEMENT_3D('',#7579,#6044,#6045);
#5238=AXIS2_PLACEMENT_3D('',#7585,#6049,#6050);
#5239=AXIS2_PLACEMENT_3D('',#7587,#6052,#6053);
#5240=AXIS2_PLACEMENT_3D('',#7588,#6054,#6055);
#5241=AXIS2_PLACEMENT_3D('',#7589,#6056,#6057);
#5242=AXIS2_PLACEMENT_3D('',#7590,#6058,#6059);
#5243=AXIS2_PLACEMENT_3D('',#7591,#6060,#6061);
#5244=AXIS2_PLACEMENT_3D('',#7594,#6062,#6063);
#5245=AXIS2_PLACEMENT_3D('',#7595,#6064,#6065);
#5246=AXIS2_PLACEMENT_3D('',#7597,#6066,#6067);
#5247=AXIS2_PLACEMENT_3D('',#7598,#6068,#6069);
#5248=AXIS2_PLACEMENT_3D('',#7602,#6071,#6072);
#5249=AXIS2_PLACEMENT_3D('',#7604,#6074,#6075);
#5250=AXIS2_PLACEMENT_3D('',#7607,#6076,#6077);
#5251=AXIS2_PLACEMENT_3D('',#7608,#6078,#6079);
#5252=AXIS2_PLACEMENT_3D('',#7610,#6080,#6081);
#5253=AXIS2_PLACEMENT_3D('',#7611,#6082,#6083);
#5254=AXIS2_PLACEMENT_3D('',#7615,#6085,#6086);
#5255=AXIS2_PLACEMENT_3D('',#7617,#6088,#6089);
#5256=AXIS2_PLACEMENT_3D('',#7620,#6090,#6091);
#5257=AXIS2_PLACEMENT_3D('',#7621,#6092,#6093);
#5258=AXIS2_PLACEMENT_3D('',#7623,#6094,#6095);
#5259=AXIS2_PLACEMENT_3D('',#7624,#6096,#6097);
#5260=AXIS2_PLACEMENT_3D('',#7628,#6099,#6100);
#5261=AXIS2_PLACEMENT_3D('',#7630,#6102,#6103);
#5262=AXIS2_PLACEMENT_3D('',#7631,#6104,#6105);
#5263=AXIS2_PLACEMENT_3D('',#7633,#6106,#6107);
#5264=AXIS2_PLACEMENT_3D('',#7636,#6109,#6110);
#5265=AXIS2_PLACEMENT_3D('',#7637,#6111,#6112);
#5266=AXIS2_PLACEMENT_3D('',#7638,#6113,#6114);
#5267=AXIS2_PLACEMENT_3D('',#7639,#6115,#6116);
#5268=AXIS2_PLACEMENT_3D('',#7641,#6117,#6118);
#5269=AXIS2_PLACEMENT_3D('',#7643,#6120,#6121);
#5270=AXIS2_PLACEMENT_3D('',#7645,#6122,#6123);
#5271=AXIS2_PLACEMENT_3D('',#7647,#6125,#6126);
#5272=AXIS2_PLACEMENT_3D('',#7649,#6127,#6128);
#5273=AXIS2_PLACEMENT_3D('',#7651,#6130,#6131);
#5274=AXIS2_PLACEMENT_3D('',#7653,#6132,#6133);
#5275=AXIS2_PLACEMENT_3D('',#7656,#6135,#6136);
#5276=AXIS2_PLACEMENT_3D('',#7657,#6137,#6138);
#5277=AXIS2_PLACEMENT_3D('',#7658,#6139,#6140);
#5278=AXIS2_PLACEMENT_3D('',#7659,#6141,#6142);
#5279=AXIS2_PLACEMENT_3D('',#7660,#6143,#6144);
#5280=AXIS2_PLACEMENT_3D('',#7662,#6145,#6146);
#5281=AXIS2_PLACEMENT_3D('',#7665,#6148,#6149);
#5282=AXIS2_PLACEMENT_3D('',#7666,#6150,#6151);
#5283=AXIS2_PLACEMENT_3D('',#7668,#6152,#6153);
#5284=AXIS2_PLACEMENT_3D('',#7671,#6155,#6156);
#5285=AXIS2_PLACEMENT_3D('',#7672,#6157,#6158);
#5286=AXIS2_PLACEMENT_3D('',#7674,#6159,#6160);
#5287=AXIS2_PLACEMENT_3D('',#7677,#6162,#6163);
#5288=AXIS2_PLACEMENT_3D('',#7678,#6164,#6165);
#5289=AXIS2_PLACEMENT_3D('',#7680,#6166,#6167);
#5290=AXIS2_PLACEMENT_3D('',#7683,#6169,#6170);
#5291=AXIS2_PLACEMENT_3D('',#7684,#6171,#6172);
#5292=AXIS2_PLACEMENT_3D('',#7686,#6173,#6174);
#5293=AXIS2_PLACEMENT_3D('',#7687,#6175,#6176);
#5294=AXIS2_PLACEMENT_3D('',#7690,#6178,#6179);
#5295=AXIS2_PLACEMENT_3D('',#7691,#6180,#6181);
#5296=AXIS2_PLACEMENT_3D('',#7699,#6185,#6186);
#5297=AXIS2_PLACEMENT_3D('',#7700,#6187,#6188);
#5298=AXIS2_PLACEMENT_3D('',#7706,#6192,#6193);
#5299=AXIS2_PLACEMENT_3D('',#7712,#6197,#6198);
#5300=AXIS2_PLACEMENT_3D('',#7714,#6200,#6201);
#5301=AXIS2_PLACEMENT_3D('',#7715,#6202,#6203);
#5302=AXIS2_PLACEMENT_3D('',#7716,#6204,#6205);
#5303=AXIS2_PLACEMENT_3D('',#7717,#6206,#6207);
#5304=AXIS2_PLACEMENT_3D('',#7718,#6208,#6209);
#5305=AXIS2_PLACEMENT_3D('',#7723,#6211,#6212);
#5306=AXIS2_PLACEMENT_3D('',#7726,#6214,#6215);
#5307=AXIS2_PLACEMENT_3D('',#7727,#6216,#6217);
#5308=AXIS2_PLACEMENT_3D('',#7728,#6218,#6219);
#5309=AXIS2_PLACEMENT_3D('',#7730,#6220,#6221);
#5310=AXIS2_PLACEMENT_3D('',#7731,#6222,#6223);
#5311=AXIS2_PLACEMENT_3D('',#7736,#6225,#6226);
#5312=AXIS2_PLACEMENT_3D('',#7739,#6228,#6229);
#5313=AXIS2_PLACEMENT_3D('',#7740,#6230,#6231);
#5314=AXIS2_PLACEMENT_3D('',#7741,#6232,#6233);
#5315=AXIS2_PLACEMENT_3D('',#7743,#6234,#6235);
#5316=AXIS2_PLACEMENT_3D('',#7744,#6236,#6237);
#5317=AXIS2_PLACEMENT_3D('',#7749,#6239,#6240);
#5318=AXIS2_PLACEMENT_3D('',#7752,#6242,#6243);
#5319=AXIS2_PLACEMENT_3D('',#7753,#6244,#6245);
#5320=AXIS2_PLACEMENT_3D('',#7754,#6246,#6247);
#5321=AXIS2_PLACEMENT_3D('',#7756,#6248,#6249);
#5322=AXIS2_PLACEMENT_3D('',#7757,#6250,#6251);
#5323=AXIS2_PLACEMENT_3D('',#7758,#6252,#6253);
#5324=AXIS2_PLACEMENT_3D('',#7760,#6254,#6255);
#5325=AXIS2_PLACEMENT_3D('',#7761,#6256,#6257);
#5326=AXIS2_PLACEMENT_3D('',#7762,#6258,#6259);
#5327=AXIS2_PLACEMENT_3D('',#7764,#6260,#6261);
#5328=AXIS2_PLACEMENT_3D('',#7765,#6262,#6263);
#5329=AXIS2_PLACEMENT_3D('',#7768,#6265,#6266);
#5330=AXIS2_PLACEMENT_3D('',#7769,#6267,#6268);
#5331=AXIS2_PLACEMENT_3D('',#7772,#6270,#6271);
#5332=AXIS2_PLACEMENT_3D('',#7773,#6272,#6273);
#5333=AXIS2_PLACEMENT_3D('',#7776,#6275,#6276);
#5334=AXIS2_PLACEMENT_3D('',#7777,#6277,#6278);
#5335=AXIS2_PLACEMENT_3D('',#7779,#6279,#6280);
#5336=AXIS2_PLACEMENT_3D('',#7781,#6282,#6283);
#5337=AXIS2_PLACEMENT_3D('',#7783,#6284,#6285);
#5338=AXIS2_PLACEMENT_3D('',#7785,#6287,#6288);
#5339=AXIS2_PLACEMENT_3D('',#7786,#6289,#6290);
#5340=AXIS2_PLACEMENT_3D('',#7787,#6291,#6292);
#5341=AXIS2_PLACEMENT_3D('',#7789,#6293,#6294);
#5342=AXIS2_PLACEMENT_3D('',#7792,#6296,#6297);
#5343=AXIS2_PLACEMENT_3D('',#7793,#6298,#6299);
#5344=AXIS2_PLACEMENT_3D('',#7802,#6304,#6305);
#5345=AXIS2_PLACEMENT_3D('',#7808,#6309,#6310);
#5346=AXIS2_PLACEMENT_3D('',#7824,#6319,#6320);
#5347=AXIS2_PLACEMENT_3D('',#7828,#6323,#6324);
#5348=AXIS2_PLACEMENT_3D('',#7832,#6327,#6328);
#5349=AXIS2_PLACEMENT_3D('',#7836,#6331,#6332);
#5350=AXIS2_PLACEMENT_3D('',#7840,#6335,#6336);
#5351=AXIS2_PLACEMENT_3D('',#7844,#6339,#6340);
#5352=AXIS2_PLACEMENT_3D('',#7848,#6343,#6344);
#5353=AXIS2_PLACEMENT_3D('',#7852,#6347,#6348);
#5354=AXIS2_PLACEMENT_3D('',#7854,#6350,#6351);
#5355=AXIS2_PLACEMENT_3D('',#7855,#6352,#6353);
#5356=AXIS2_PLACEMENT_3D('',#7856,#6354,#6355);
#5357=AXIS2_PLACEMENT_3D('',#7859,#6356,#6357);
#5358=AXIS2_PLACEMENT_3D('',#7860,#6358,#6359);
#5359=AXIS2_PLACEMENT_3D('',#7861,#6360,#6361);
#5360=AXIS2_PLACEMENT_3D('',#7863,#6362,#6363);
#5361=AXIS2_PLACEMENT_3D('',#7865,#6364,#6365);
#5362=AXIS2_PLACEMENT_3D('',#7866,#6366,#6367);
#5363=AXIS2_PLACEMENT_3D('',#7868,#6368,#6369);
#5364=AXIS2_PLACEMENT_3D('',#7870,#6371,#6372);
#5365=AXIS2_PLACEMENT_3D('',#7873,#6374,#6375);
#5366=AXIS2_PLACEMENT_3D('',#7874,#6376,#6377);
#5367=AXIS2_PLACEMENT_3D('',#7875,#6378,#6379);
#5368=AXIS2_PLACEMENT_3D('',#7876,#6380,#6381);
#5369=AXIS2_PLACEMENT_3D('',#7877,#6382,#6383);
#5370=AXIS2_PLACEMENT_3D('',#7879,#6384,#6385);
#5371=AXIS2_PLACEMENT_3D('',#7881,#6386,#6387);
#5372=AXIS2_PLACEMENT_3D('',#7882,#6388,#6389);
#5373=AXIS2_PLACEMENT_3D('',#7885,#6391,#6392);
#5374=AXIS2_PLACEMENT_3D('',#7886,#6393,#6394);
#5375=AXIS2_PLACEMENT_3D('',#7888,#6395,#6396);
#5376=AXIS2_PLACEMENT_3D('',#7889,#6397,#6398);
#5377=AXIS2_PLACEMENT_3D('',#7891,#6399,#6400);
#5378=AXIS2_PLACEMENT_3D('',#7893,#6402,#6403);
#5379=AXIS2_PLACEMENT_3D('',#7895,#6404,#6405);
#5380=AXIS2_PLACEMENT_3D('',#7897,#6407,#6408);
#5381=AXIS2_PLACEMENT_3D('',#7898,#6409,#6410);
#5382=AXIS2_PLACEMENT_3D('',#7899,#6411,#6412);
#5383=AXIS2_PLACEMENT_3D('',#7901,#6413,#6414);
#5384=AXIS2_PLACEMENT_3D('',#7904,#6416,#6417);
#5385=AXIS2_PLACEMENT_3D('',#7905,#6418,#6419);
#5386=AXIS2_PLACEMENT_3D('',#7907,#6420,#6421);
#5387=AXIS2_PLACEMENT_3D('',#7910,#6423,#6424);
#5388=AXIS2_PLACEMENT_3D('',#7911,#6425,#6426);
#5389=AXIS2_PLACEMENT_3D('',#7912,#6427,#6428);
#5390=AXIS2_PLACEMENT_3D('',#7913,#6429,#6430);
#5391=AXIS2_PLACEMENT_3D('',#8565,#6431,#6432);
#5392=AXIS2_PLACEMENT_3D('',#8632,#6433,#6434);
#5393=AXIS2_PLACEMENT_3D('',#8633,#6435,#6436);
#5394=AXIS2_PLACEMENT_3D('',#8634,#6437,#6438);
#5395=AXIS2_PLACEMENT_3D('',#8635,#6439,#6440);
#5396=AXIS2_PLACEMENT_3D('',#8636,#6441,#6442);
#5397=AXIS2_PLACEMENT_3D('',#8645,#6447,#6448);
#5398=AXIS2_PLACEMENT_3D('',#8651,#6452,#6453);
#5399=AXIS2_PLACEMENT_3D('',#8657,#6457,#6458);
#5400=AXIS2_PLACEMENT_3D('',#8660,#6461,#6462);
#5401=AXIS2_PLACEMENT_3D('',#8661,#6463,#6464);
#5402=AXIS2_PLACEMENT_3D('',#8662,#6465,#6466);
#5403=AXIS2_PLACEMENT_3D('',#8663,#6467,#6468);
#5404=AXIS2_PLACEMENT_3D('',#8672,#6473,#6474);
#5405=AXIS2_PLACEMENT_3D('',#8678,#6478,#6479);
#5406=AXIS2_PLACEMENT_3D('',#8684,#6483,#6484);
#5407=AXIS2_PLACEMENT_3D('',#8687,#6487,#6488);
#5408=AXIS2_PLACEMENT_3D('',#8688,#6489,#6490);
#5409=AXIS2_PLACEMENT_3D('',#8689,#6491,#6492);
#5410=AXIS2_PLACEMENT_3D('',#8690,#6493,#6494);
#5411=AXIS2_PLACEMENT_3D('',#8692,#6495,#6496);
#5412=AXIS2_PLACEMENT_3D('',#8695,#6498,#6499);
#5413=AXIS2_PLACEMENT_3D('',#8696,#6500,#6501);
#5414=AXIS2_PLACEMENT_3D('',#8698,#6502,#6503);
#5415=AXIS2_PLACEMENT_3D('',#8701,#6505,#6506);
#5416=AXIS2_PLACEMENT_3D('',#8702,#6507,#6508);
#5417=AXIS2_PLACEMENT_3D('',#8703,#6509,#6510);
#5418=AXIS2_PLACEMENT_3D('',#8704,#6511,#6512);
#5419=AXIS2_PLACEMENT_3D('',#8705,#6513,#6514);
#5420=AXIS2_PLACEMENT_3D('',#8714,#6519,#6520);
#5421=AXIS2_PLACEMENT_3D('',#8720,#6524,#6525);
#5422=AXIS2_PLACEMENT_3D('',#8726,#6529,#6530);
#5423=AXIS2_PLACEMENT_3D('',#8732,#6534,#6535);
#5424=AXIS2_PLACEMENT_3D('',#8738,#6539,#6540);
#5425=AXIS2_PLACEMENT_3D('',#8741,#6543,#6544);
#5426=AXIS2_PLACEMENT_3D('',#8742,#6545,#6546);
#5427=AXIS2_PLACEMENT_3D('',#8743,#6547,#6548);
#5428=AXIS2_PLACEMENT_3D('',#8745,#6549,#6550);
#5429=AXIS2_PLACEMENT_3D('',#8746,#6551,#6552);
#5430=AXIS2_PLACEMENT_3D('',#8748,#6553,#6554);
#5431=AXIS2_PLACEMENT_3D('',#8749,#6555,#6556);
#5432=AXIS2_PLACEMENT_3D('',#8751,#6557,#6558);
#5433=AXIS2_PLACEMENT_3D('',#8753,#6560,#6561);
#5434=AXIS2_PLACEMENT_3D('',#8755,#6562,#6563);
#5435=AXIS2_PLACEMENT_3D('',#8757,#6565,#6566);
#5436=AXIS2_PLACEMENT_3D('',#8759,#6567,#6568);
#5437=AXIS2_PLACEMENT_3D('',#8761,#6570,#6571);
#5438=AXIS2_PLACEMENT_3D('',#8763,#6572,#6573);
#5439=AXIS2_PLACEMENT_3D('',#8764,#6574,#6575);
#5440=AXIS2_PLACEMENT_3D('',#8766,#6576,#6577);
#5441=AXIS2_PLACEMENT_3D('',#8768,#6579,#6580);
#5442=AXIS2_PLACEMENT_3D('',#8770,#6582,#6583);
#5443=AXIS2_PLACEMENT_3D('',#8771,#6584,#6585);
#5444=AXIS2_PLACEMENT_3D('',#8772,#6586,#6587);
#5445=AXIS2_PLACEMENT_3D('',#8775,#6588,#6589);
#5446=AXIS2_PLACEMENT_3D('',#8776,#6590,#6591);
#5447=AXIS2_PLACEMENT_3D('',#8778,#6592,#6593);
#5448=AXIS2_PLACEMENT_3D('',#8780,#6594,#6595);
#5449=AXIS2_PLACEMENT_3D('',#8781,#6596,#6597);
#5450=AXIS2_PLACEMENT_3D('',#8782,#6598,#6599);
#5451=AXIS2_PLACEMENT_3D('',#8785,#6601,#6602);
#5452=AXIS2_PLACEMENT_3D('',#8786,#6603,#6604);
#5453=AXIS2_PLACEMENT_3D('',#8788,#6605,#6606);
#5454=AXIS2_PLACEMENT_3D('',#8791,#6608,#6609);
#5455=AXIS2_PLACEMENT_3D('',#8792,#6610,#6611);
#5456=AXIS2_PLACEMENT_3D('',#8795,#6613,#6614);
#5457=AXIS2_PLACEMENT_3D('',#8796,#6615,#6616);
#5458=AXIS2_PLACEMENT_3D('',#8797,#6617,#6618);
#5459=AXIS2_PLACEMENT_3D('',#8799,#6619,#6620);
#5460=AXIS2_PLACEMENT_3D('',#8801,#6622,#6623);
#5461=AXIS2_PLACEMENT_3D('',#8803,#6624,#6625);
#5462=AXIS2_PLACEMENT_3D('',#8804,#6626,#6627);
#5463=AXIS2_PLACEMENT_3D('',#8806,#6629,#6630);
#5464=AXIS2_PLACEMENT_3D('',#8807,#6631,#6632);
#5465=AXIS2_PLACEMENT_3D('',#8810,#6633,#6634);
#5466=AXIS2_PLACEMENT_3D('',#8811,#6635,#6636);
#5467=AXIS2_PLACEMENT_3D('',#8813,#6637,#6638);
#5468=AXIS2_PLACEMENT_3D('',#8815,#6639,#6640);
#5469=AXIS2_PLACEMENT_3D('',#8816,#6641,#6642);
#5470=AXIS2_PLACEMENT_3D('',#8817,#6643,#6644);
#5471=AXIS2_PLACEMENT_3D('',#8819,#6645,#6646);
#5472=AXIS2_PLACEMENT_3D('',#8821,#6648,#6649);
#5473=AXIS2_PLACEMENT_3D('',#8823,#6650,#6651);
#5474=AXIS2_PLACEMENT_3D('',#8825,#6652,#6653);
#5475=AXIS2_PLACEMENT_3D('',#8826,#6654,#6655);
#5476=AXIS2_PLACEMENT_3D('',#8828,#6656,#6657);
#5477=AXIS2_PLACEMENT_3D('',#8830,#6659,#6660);
#5478=AXIS2_PLACEMENT_3D('',#8832,#6661,#6662);
#5479=AXIS2_PLACEMENT_3D('',#8834,#6664,#6665);
#5480=AXIS2_PLACEMENT_3D('',#8836,#6666,#6667);
#5481=AXIS2_PLACEMENT_3D('',#8838,#6669,#6670);
#5482=AXIS2_PLACEMENT_3D('',#8839,#6671,#6672);
#5483=AXIS2_PLACEMENT_3D('',#8841,#6674,#6675);
#5484=AXIS2_PLACEMENT_3D('',#8842,#6676,#6677);
#5485=AXIS2_PLACEMENT_3D('',#8845,#6678,#6679);
#5486=AXIS2_PLACEMENT_3D('',#8846,#6680,#6681);
#5487=AXIS2_PLACEMENT_3D('',#8849,#6682,#6683);
#5488=AXIS2_PLACEMENT_3D('',#8850,#6684,#6685);
#5489=AXIS2_PLACEMENT_3D('',#8853,#6686,#6687);
#5490=AXIS2_PLACEMENT_3D('',#8854,#6688,#6689);
#5491=AXIS2_PLACEMENT_3D('',#8857,#6690,#6691);
#5492=AXIS2_PLACEMENT_3D('',#8858,#6692,#6693);
#5493=AXIS2_PLACEMENT_3D('',#8861,#6694,#6695);
#5494=AXIS2_PLACEMENT_3D('',#8862,#6696,#6697);
#5495=AXIS2_PLACEMENT_3D('',#8865,#6698,#6699);
#5496=AXIS2_PLACEMENT_3D('',#8866,#6700,#6701);
#5497=AXIS2_PLACEMENT_3D('',#8869,#6702,#6703);
#5498=AXIS2_PLACEMENT_3D('',#8870,#6704,#6705);
#5499=AXIS2_PLACEMENT_3D('',#8873,#6706,#6707);
#5500=AXIS2_PLACEMENT_3D('',#8874,#6708,#6709);
#5501=AXIS2_PLACEMENT_3D('',#8875,#6710,#6711);
#5502=AXIS2_PLACEMENT_3D('',#8901,#6712,#6713);
#5503=AXIS2_PLACEMENT_3D('',#8925,#6714,#6715);
#5504=AXIS2_PLACEMENT_3D('',#8926,#6716,#6717);
#5505=AXIS2_PLACEMENT_3D('',#8928,#6718,#6719);
#5506=AXIS2_PLACEMENT_3D('',#8953,#6720,#6721);
#5507=AXIS2_PLACEMENT_3D('',#8978,#6722,#6723);
#5508=AXIS2_PLACEMENT_3D('',#8994,#6725,#6726);
#5509=AXIS2_PLACEMENT_3D('',#9009,#6727,#6728);
#5510=AXIS2_PLACEMENT_3D('',#9034,#6729,#6730);
#5511=AXIS2_PLACEMENT_3D('',#9059,#6731,#6732);
#5512=AXIS2_PLACEMENT_3D('',#9084,#6733,#6734);
#5513=AXIS2_PLACEMENT_3D('',#9108,#6735,#6736);
#5514=AXIS2_PLACEMENT_3D('',#9109,#6737,#6738);
#5515=AXIS2_PLACEMENT_3D('',#9111,#6739,#6740);
#5516=AXIS2_PLACEMENT_3D('',#9112,#6741,#6742);
#5517=AXIS2_PLACEMENT_3D('',#9113,#6743,#6744);
#5518=AXIS2_PLACEMENT_3D('',#9137,#6745,#6746);
#5519=AXIS2_PLACEMENT_3D('',#9138,#6747,#6748);
#5520=AXIS2_PLACEMENT_3D('',#9140,#6749,#6750);
#5521=AXIS2_PLACEMENT_3D('',#9141,#6751,#6752);
#5522=AXIS2_PLACEMENT_3D('',#9142,#6753,#6754);
#5523=AXIS2_PLACEMENT_3D('',#9166,#6755,#6756);
#5524=AXIS2_PLACEMENT_3D('',#9167,#6757,#6758);
#5525=AXIS2_PLACEMENT_3D('',#9169,#6759,#6760);
#5526=AXIS2_PLACEMENT_3D('',#9170,#6761,#6762);
#5527=AXIS2_PLACEMENT_3D('',#9171,#6763,#6764);
#5528=AXIS2_PLACEMENT_3D('',#9186,#6765,#6766);
#5529=AXIS2_PLACEMENT_3D('',#9199,#6767,#6768);
#5530=AXIS2_PLACEMENT_3D('',#9201,#6769,#6770);
#5531=AXIS2_PLACEMENT_3D('',#9202,#6771,#6772);
#5532=AXIS2_PLACEMENT_3D('',#9203,#6773,#6774);
#5533=AXIS2_PLACEMENT_3D('',#9227,#6775,#6776);
#5534=AXIS2_PLACEMENT_3D('',#9228,#6777,#6778);
#5535=AXIS2_PLACEMENT_3D('',#9230,#6779,#6780);
#5536=AXIS2_PLACEMENT_3D('',#9231,#6781,#6782);
#5537=AXIS2_PLACEMENT_3D('',#9232,#6783,#6784);
#5538=AXIS2_PLACEMENT_3D('',#9256,#6785,#6786);
#5539=AXIS2_PLACEMENT_3D('',#9257,#6787,#6788);
#5540=AXIS2_PLACEMENT_3D('',#9259,#6789,#6790);
#5541=AXIS2_PLACEMENT_3D('',#9260,#6791,#6792);
#5542=AXIS2_PLACEMENT_3D('',#9261,#6793,#6794);
#5543=AXIS2_PLACEMENT_3D('',#9285,#6795,#6796);
#5544=AXIS2_PLACEMENT_3D('',#9286,#6797,#6798);
#5545=AXIS2_PLACEMENT_3D('',#9288,#6799,#6800);
#5546=AXIS2_PLACEMENT_3D('',#9291,#6802,#6803);
#5547=AXIS2_PLACEMENT_3D('',#9315,#6804,#6805);
#5548=AXIS2_PLACEMENT_3D('',#9316,#6806,#6807);
#5549=AXIS2_PLACEMENT_3D('',#9317,#6808,#6809);
#5550=AXIS2_PLACEMENT_3D('',#9318,#6810,#6811);
#5551=AXIS2_PLACEMENT_3D('',#9319,#6812,#6813);
#5552=AXIS2_PLACEMENT_3D('',#9320,#6814,#6815);
#5553=AXIS2_PLACEMENT_3D('',#9321,#6816,#6817);
#5554=AXIS2_PLACEMENT_3D('',#9322,#6818,#6819);
#5555=AXIS2_PLACEMENT_3D('',#9323,#6820,#6821);
#5556=AXIS2_PLACEMENT_3D('',#9325,#6822,#6823);
#5557=AXIS2_PLACEMENT_3D('',#9327,#6824,#6825);
#5558=AXIS2_PLACEMENT_3D('',#9328,#6826,#6827);
#5559=AXIS2_PLACEMENT_3D('',#9330,#6828,#6829);
#5560=AXIS2_PLACEMENT_3D('',#9332,#6831,#6832);
#5561=AXIS2_PLACEMENT_3D('',#9334,#6833,#6834);
#5562=AXIS2_PLACEMENT_3D('',#9335,#6835,#6836);
#5563=AXIS2_PLACEMENT_3D('',#9337,#6838,#6839);
#5564=AXIS2_PLACEMENT_3D('',#9339,#6840,#6841);
#5565=AXIS2_PLACEMENT_3D('',#9341,#6842,#6843);
#5566=AXIS2_PLACEMENT_3D('',#9342,#6844,#6845);
#5567=AXIS2_PLACEMENT_3D('',#9344,#6846,#6847);
#5568=AXIS2_PLACEMENT_3D('',#9346,#6849,#6850);
#5569=AXIS2_PLACEMENT_3D('',#9348,#6851,#6852);
#5570=AXIS2_PLACEMENT_3D('',#9349,#6853,#6854);
#5571=AXIS2_PLACEMENT_3D('',#9351,#6856,#6857);
#5572=AXIS2_PLACEMENT_3D('',#9352,#6858,#6859);
#5573=AXIS2_PLACEMENT_3D('',#9353,#6860,#6861);
#5574=AXIS2_PLACEMENT_3D('',#9354,#6862,#6863);
#5575=AXIS2_PLACEMENT_3D('',#9355,#6864,#6865);
#5576=AXIS2_PLACEMENT_3D('',#9356,#6866,#6867);
#5577=AXIS2_PLACEMENT_3D('',#9357,#6868,#6869);
#5578=AXIS2_PLACEMENT_3D('',#9366,#6874,#6875);
#5579=AXIS2_PLACEMENT_3D('',#9372,#6879,#6880);
#5580=AXIS2_PLACEMENT_3D('',#9378,#6884,#6885);
#5581=AXIS2_PLACEMENT_3D('',#9384,#6889,#6890);
#5582=AXIS2_PLACEMENT_3D('',#9390,#6894,#6895);
#5583=AXIS2_PLACEMENT_3D('',#9393,#6898,#6899);
#5584=AXIS2_PLACEMENT_3D('',#9394,#6900,#6901);
#5585=AXIS2_PLACEMENT_3D('',#9395,#6902,#6903);
#5586=AXIS2_PLACEMENT_3D('',#9397,#6904,#6905);
#5587=AXIS2_PLACEMENT_3D('',#9398,#6906,#6907);
#5588=AXIS2_PLACEMENT_3D('',#9400,#6908,#6909);
#5589=AXIS2_PLACEMENT_3D('',#9401,#6910,#6911);
#5590=AXIS2_PLACEMENT_3D('',#9403,#6912,#6913);
#5591=AXIS2_PLACEMENT_3D('',#9405,#6915,#6916);
#5592=AXIS2_PLACEMENT_3D('',#9407,#6917,#6918);
#5593=AXIS2_PLACEMENT_3D('',#9409,#6920,#6921);
#5594=AXIS2_PLACEMENT_3D('',#9411,#6922,#6923);
#5595=AXIS2_PLACEMENT_3D('',#9413,#6925,#6926);
#5596=AXIS2_PLACEMENT_3D('',#9415,#6927,#6928);
#5597=AXIS2_PLACEMENT_3D('',#9416,#6929,#6930);
#5598=AXIS2_PLACEMENT_3D('',#9418,#6931,#6932);
#5599=AXIS2_PLACEMENT_3D('',#9420,#6934,#6935);
#5600=AXIS2_PLACEMENT_3D('',#9422,#6937,#6938);
#5601=AXIS2_PLACEMENT_3D('',#9423,#6939,#6940);
#5602=AXIS2_PLACEMENT_3D('',#9424,#6941,#6942);
#5603=AXIS2_PLACEMENT_3D('',#9425,#6943,#6944);
#5604=AXIS2_PLACEMENT_3D('',#9426,#6945,#6946);
#5605=AXIS2_PLACEMENT_3D('',#9427,#6947,#6948);
#5606=AXIS2_PLACEMENT_3D('',#9428,#6949,#6950);
#5607=AXIS2_PLACEMENT_3D('',#9429,#6951,#6952);
#5608=AXIS2_PLACEMENT_3D('',#9430,#6953,#6954);
#5609=AXIS2_PLACEMENT_3D('',#9431,#6955,#6956);
#5610=AXIS2_PLACEMENT_3D('',#9432,#6957,#6958);
#5611=AXIS2_PLACEMENT_3D('',#9433,#6959,#6960);
#5612=AXIS2_PLACEMENT_3D('',#9434,#6961,#6962);
#5613=AXIS2_PLACEMENT_3D('',#9435,#6963,#6964);
#5614=AXIS2_PLACEMENT_3D('',#9436,#6965,#6966);
#5615=AXIS2_PLACEMENT_3D('',#9437,#6967,#6968);
#5616=AXIS2_PLACEMENT_3D('',#9438,#6969,#6970);
#5617=AXIS2_PLACEMENT_3D('',#9439,#6971,#6972);
#5618=AXIS2_PLACEMENT_3D('',#9440,#6973,#6974);
#5619=AXIS2_PLACEMENT_3D('',#9441,#6975,#6976);
#5620=AXIS2_PLACEMENT_3D('',#9442,#6977,#6978);
#5621=AXIS2_PLACEMENT_3D('',#9443,#6979,#6980);
#5622=AXIS2_PLACEMENT_3D('',#9444,#6981,#6982);
#5623=AXIS2_PLACEMENT_3D('',#9445,#6983,#6984);
#5624=AXIS2_PLACEMENT_3D('',#9446,#6985,#6986);
#5625=AXIS2_PLACEMENT_3D('',#9447,#6987,#6988);
#5626=AXIS2_PLACEMENT_3D('',#9448,#6989,#6990);
#5627=AXIS2_PLACEMENT_3D('',#9449,#6991,#6992);
#5628=AXIS2_PLACEMENT_3D('',#9450,#6993,#6994);
#5629=AXIS2_PLACEMENT_3D('',#9451,#6995,#6996);
#5630=AXIS2_PLACEMENT_3D('',#9452,#6997,#6998);
#5631=AXIS2_PLACEMENT_3D('',#9453,#6999,#7000);
#5632=AXIS2_PLACEMENT_3D('',#9454,#7001,#7002);
#5633=AXIS2_PLACEMENT_3D('',#9455,#7003,#7004);
#5634=AXIS2_PLACEMENT_3D('',#9456,#7005,#7006);
#5635=AXIS2_PLACEMENT_3D('',#9457,#7007,#7008);
#5636=AXIS2_PLACEMENT_3D('',#9459,#7009,#7010);
#5637=AXIS2_PLACEMENT_3D('',#9462,#7012,#7013);
#5638=AXIS2_PLACEMENT_3D('',#9463,#7014,#7015);
#5639=AXIS2_PLACEMENT_3D('',#9464,#7016,#7017);
#5640=AXIS2_PLACEMENT_3D('',#9466,#7018,#7019);
#5641=AXIS2_PLACEMENT_3D('',#9469,#7021,#7022);
#5642=AXIS2_PLACEMENT_3D('',#9470,#7023,#7024);
#5643=AXIS2_PLACEMENT_3D('',#9471,#7025,#7026);
#5644=AXIS2_PLACEMENT_3D('',#9515,#7027,#7028);
#5645=AXIS2_PLACEMENT_3D('',#9520,#7030,#7031);
#5646=AXIS2_PLACEMENT_3D('',#9523,#7033,#7034);
#5647=AXIS2_PLACEMENT_3D('',#9524,#7035,#7036);
#5648=AXIS2_PLACEMENT_3D('',#9529,#7039,#7040);
#5649=AXIS2_PLACEMENT_3D('',#9530,#7041,#7042);
#5650=AXIS2_PLACEMENT_3D('',#9535,#7045,#7046);
#5651=AXIS2_PLACEMENT_3D('',#9536,#7047,#7048);
#5652=AXIS2_PLACEMENT_3D('',#9547,#7054,#7055);
#5653=AXIS2_PLACEMENT_3D('',#9549,#7056,#7057);
#5654=AXIS2_PLACEMENT_3D('',#9551,#7058,#7059);
#5655=AXIS2_PLACEMENT_3D('',#9553,#7060,#7061);
#5656=AXIS2_PLACEMENT_3D('',#9554,#7062,#7063);
#5657=AXIS2_PLACEMENT_3D('',#9557,#7065,#7066);
#5658=AXIS2_PLACEMENT_3D('',#9558,#7067,#7068);
#5659=AXIS2_PLACEMENT_3D('',#9561,#7070,#7071);
#5660=AXIS2_PLACEMENT_3D('',#9562,#7072,#7073);
#5661=AXIS2_PLACEMENT_3D('',#9565,#7075,#7076);
#5662=AXIS2_PLACEMENT_3D('',#9566,#7077,#7078);
#5663=AXIS2_PLACEMENT_3D('',#9569,#7080,#7081);
#5664=AXIS2_PLACEMENT_3D('',#9570,#7082,#7083);
#5665=AXIS2_PLACEMENT_3D('',#9573,#7085,#7086);
#5666=AXIS2_PLACEMENT_3D('',#9574,#7087,#7088);
#5667=AXIS2_PLACEMENT_3D('',#9582,#7093,#7094);
#5668=AXIS2_PLACEMENT_3D('',#9585,#7097,#7098);
#5669=AXIS2_PLACEMENT_3D('',#9586,#7099,#7100);
#5670=AXIS2_PLACEMENT_3D('',#9587,#7101,#7102);
#5671=AXIS2_PLACEMENT_3D('',#9589,#7103,#7104);
#5672=AXIS2_PLACEMENT_3D('',#9590,#7105,#7106);
#5673=AXIS2_PLACEMENT_3D('',#9592,#7107,#7108);
#5674=AXIS2_PLACEMENT_3D('',#9593,#7109,#7110);
#5675=AXIS2_PLACEMENT_3D('',#9596,#7112,#7113);
#5676=AXIS2_PLACEMENT_3D('',#9597,#7114,#7115);
#5677=AXIS2_PLACEMENT_3D('',#9599,#7116,#7117);
#5678=AXIS2_PLACEMENT_3D('',#9601,#7119,#7120);
#5679=AXIS2_PLACEMENT_3D('',#9602,#7121,#7122);
#5680=AXIS2_PLACEMENT_3D('',#9603,#7123,#7124);
#5681=AXIS2_PLACEMENT_3D('',#9604,#7125,#7126);
#5682=AXIS2_PLACEMENT_3D('',#9606,#7127,#7128);
#5683=AXIS2_PLACEMENT_3D('',#9609,#7130,#7131);
#5684=AXIS2_PLACEMENT_3D('',#9610,#7132,#7133);
#5685=AXIS2_PLACEMENT_3D('',#9612,#7134,#7135);
#5686=AXIS2_PLACEMENT_3D('',#9615,#7137,#7138);
#5687=AXIS2_PLACEMENT_3D('',#9616,#7139,#7140);
#5688=AXIS2_PLACEMENT_3D('',#9617,#7141,#7142);
#5689=AXIS2_PLACEMENT_3D('',#9618,#7143,#7144);
#5690=AXIS2_PLACEMENT_3D('',#9619,#7145,#7146);
#5691=AXIS2_PLACEMENT_3D('',#9621,#7147,#7148);
#5692=AXIS2_PLACEMENT_3D('',#9624,#7150,#7151);
#5693=AXIS2_PLACEMENT_3D('',#9625,#7152,#7153);
#5694=AXIS2_PLACEMENT_3D('',#9627,#7154,#7155);
#5695=AXIS2_PLACEMENT_3D('',#9630,#7157,#7158);
#5696=AXIS2_PLACEMENT_3D('',#9631,#7159,#7160);
#5697=AXIS2_PLACEMENT_3D('',#9632,#7161,#7162);
#5698=AXIS2_PLACEMENT_3D('',#9633,#7163,#7164);
#5699=AXIS2_PLACEMENT_3D('',#9634,#7165,#7166);
#5700=AXIS2_PLACEMENT_3D('',#9636,#7167,#7168);
#5701=AXIS2_PLACEMENT_3D('',#9639,#7170,#7171);
#5702=AXIS2_PLACEMENT_3D('',#9640,#7172,#7173);
#5703=AXIS2_PLACEMENT_3D('',#9642,#7174,#7175);
#5704=AXIS2_PLACEMENT_3D('',#9645,#7177,#7178);
#5705=AXIS2_PLACEMENT_3D('',#9646,#7179,#7180);
#5706=AXIS2_PLACEMENT_3D('',#9647,#7181,#7182);
#5707=AXIS2_PLACEMENT_3D('',#9648,#7183,#7184);
#5708=AXIS2_PLACEMENT_3D('',#9649,#7185,#7186);
#5709=AXIS2_PLACEMENT_3D('',#9651,#7187,#7188);
#5710=AXIS2_PLACEMENT_3D('',#9654,#7190,#7191);
#5711=AXIS2_PLACEMENT_3D('',#9655,#7192,#7193);
#5712=AXIS2_PLACEMENT_3D('',#9657,#7194,#7195);
#5713=AXIS2_PLACEMENT_3D('',#9660,#7197,#7198);
#5714=AXIS2_PLACEMENT_3D('',#9661,#7199,#7200);
#5715=AXIS2_PLACEMENT_3D('',#9662,#7201,#7202);
#5716=AXIS2_PLACEMENT_3D('',#9663,#7203,#7204);
#5717=AXIS2_PLACEMENT_3D('',#9664,#7205,#7206);
#5718=AXIS2_PLACEMENT_3D('',#9666,#7207,#7208);
#5719=AXIS2_PLACEMENT_3D('',#9667,#7209,#7210);
#5720=AXIS2_PLACEMENT_3D('',#9669,#7211,#7212);
#5721=AXIS2_PLACEMENT_3D('',#9671,#7214,#7215);
#5722=AXIS2_PLACEMENT_3D('',#9673,#7216,#7217);
#5723=AXIS2_PLACEMENT_3D('',#9675,#7219,#7220);
#5724=AXIS2_PLACEMENT_3D('',#9677,#7221,#7222);
#5725=AXIS2_PLACEMENT_3D('',#9679,#7224,#7225);
#5726=AXIS2_PLACEMENT_3D('',#9681,#7226,#7227);
#5727=AXIS2_PLACEMENT_3D('',#9682,#7228,#7229);
#5728=AXIS2_PLACEMENT_3D('',#9684,#7230,#7231);
#5729=AXIS2_PLACEMENT_3D('',#9686,#7233,#7234);
#5730=AXIS2_PLACEMENT_3D('',#9688,#7235,#7236);
#5731=AXIS2_PLACEMENT_3D('',#9690,#7238,#7239);
#5732=AXIS2_PLACEMENT_3D('',#9692,#7240,#7241);
#5733=AXIS2_PLACEMENT_3D('',#9694,#7243,#7244);
#5734=AXIS2_PLACEMENT_3D('',#9695,#7245,#7246);
#5735=AXIS2_PLACEMENT_3D('',#9704,#7251,#7252);
#5736=AXIS2_PLACEMENT_3D('',#9710,#7256,#7257);
#5737=AXIS2_PLACEMENT_3D('',#9716,#7261,#7262);
#5738=AXIS2_PLACEMENT_3D('',#9722,#7266,#7267);
#5739=AXIS2_PLACEMENT_3D('',#9728,#7271,#7272);
#5740=AXIS2_PLACEMENT_3D('',#9731,#7275,#7276);
#5741=AXIS2_PLACEMENT_3D('',#9732,#7277,#7278);
#5742=AXIS2_PLACEMENT_3D('',#9733,#7279,#7280);
#5743=AXIS2_PLACEMENT_3D('',#9734,#7281,#7282);
#5744=AXIS2_PLACEMENT_3D('',#9735,#7283,#7284);
#5745=AXIS2_PLACEMENT_3D('',#9736,#7285,#7286);
#5746=AXIS2_PLACEMENT_3D('',#9737,#7287,#7288);
#5747=AXIS2_PLACEMENT_3D('',#9738,#7289,#7290);
#5748=AXIS2_PLACEMENT_3D('',#9739,#7291,#7292);
#5749=AXIS2_PLACEMENT_3D('',#9740,#7293,#7294);
#5750=AXIS2_PLACEMENT_3D('',#9741,#7295,#7296);
#5751=DIRECTION('axis',(0.,0.,1.));
#5752=DIRECTION('refdir',(1.,0.,0.));
#5753=DIRECTION('axis',(0.,0.,1.));
#5754=DIRECTION('refdir',(1.,0.,0.));
#5755=DIRECTION('axis',(0.,0.,1.));
#5756=DIRECTION('refdir',(1.,0.,0.));
#5757=DIRECTION('center_axis',(0.,0.,1.));
#5758=DIRECTION('ref_axis',(1.,0.,0.));
#5759=DIRECTION('center_axis',(0.,0.,1.));
#5760=DIRECTION('ref_axis',(1.,0.,0.));
#5761=DIRECTION('',(0.,0.,1.));
#5762=DIRECTION('center_axis',(0.,0.,-1.));
#5763=DIRECTION('ref_axis',(1.,0.,0.));
#5764=DIRECTION('center_axis',(0.,0.,1.));
#5765=DIRECTION('ref_axis',(1.,0.,0.));
#5766=DIRECTION('center_axis',(0.,0.,1.));
#5767=DIRECTION('ref_axis',(1.,0.,0.));
#5768=DIRECTION('',(0.,0.,1.));
#5769=DIRECTION('center_axis',(0.,0.,-1.));
#5770=DIRECTION('ref_axis',(1.,0.,0.));
#5771=DIRECTION('center_axis',(0.,0.,1.));
#5772=DIRECTION('ref_axis',(1.,0.,0.));
#5773=DIRECTION('center_axis',(0.,0.,1.));
#5774=DIRECTION('ref_axis',(1.,0.,0.));
#5775=DIRECTION('',(0.,0.,1.));
#5776=DIRECTION('center_axis',(0.,0.,-1.));
#5777=DIRECTION('ref_axis',(1.,0.,0.));
#5778=DIRECTION('center_axis',(0.,0.,1.));
#5779=DIRECTION('ref_axis',(1.,0.,0.));
#5780=DIRECTION('center_axis',(0.,0.,1.));
#5781=DIRECTION('ref_axis',(1.,0.,0.));
#5782=DIRECTION('',(0.,0.,1.));
#5783=DIRECTION('center_axis',(0.,0.,-1.));
#5784=DIRECTION('ref_axis',(1.,0.,0.));
#5785=DIRECTION('center_axis',(0.,1.,0.));
#5786=DIRECTION('ref_axis',(-1.,0.,0.));
#5787=DIRECTION('',(-1.,0.,0.));
#5788=DIRECTION('',(0.,0.,1.));
#5789=DIRECTION('',(-1.,0.,0.));
#5790=DIRECTION('',(0.,0.,1.));
#5791=DIRECTION('center_axis',(1.,0.,0.));
#5792=DIRECTION('ref_axis',(0.,1.,0.));
#5793=DIRECTION('',(0.,1.,0.));
#5794=DIRECTION('',(0.,1.,0.));
#5795=DIRECTION('',(0.,0.,1.));
#5796=DIRECTION('center_axis',(0.,-1.,0.));
#5797=DIRECTION('ref_axis',(1.,0.,0.));
#5798=DIRECTION('',(1.,0.,0.));
#5799=DIRECTION('',(1.,0.,0.));
#5800=DIRECTION('',(0.,0.,1.));
#5801=DIRECTION('center_axis',(-1.,0.,0.));
#5802=DIRECTION('ref_axis',(0.,-1.,0.));
#5803=DIRECTION('',(0.,-1.,0.));
#5804=DIRECTION('',(0.,-1.,0.));
#5805=DIRECTION('center_axis',(0.,0.,1.));
#5806=DIRECTION('ref_axis',(1.,0.,0.));
#5807=DIRECTION('center_axis',(0.,0.,1.));
#5808=DIRECTION('ref_axis',(1.,0.,0.));
#5809=DIRECTION('axis',(0.,0.,1.));
#5810=DIRECTION('refdir',(1.,0.,0.));
#5811=DIRECTION('center_axis',(0.,1.,0.));
#5812=DIRECTION('ref_axis',(-1.,0.,0.));
#5813=DIRECTION('',(-1.,0.,0.));
#5814=DIRECTION('',(0.,0.,1.));
#5815=DIRECTION('',(-1.,0.,0.));
#5816=DIRECTION('',(0.,0.,1.));
#5817=DIRECTION('center_axis',(1.,0.,0.));
#5818=DIRECTION('ref_axis',(0.,1.,0.));
#5819=DIRECTION('',(0.,1.,0.));
#5820=DIRECTION('',(0.,1.,0.));
#5821=DIRECTION('',(0.,0.,1.));
#5822=DIRECTION('center_axis',(0.,-1.,0.));
#5823=DIRECTION('ref_axis',(1.,0.,0.));
#5824=DIRECTION('',(1.,0.,0.));
#5825=DIRECTION('',(1.,0.,0.));
#5826=DIRECTION('',(0.,0.,1.));
#5827=DIRECTION('center_axis',(-1.,0.,0.));
#5828=DIRECTION('ref_axis',(0.,-1.,0.));
#5829=DIRECTION('',(0.,-1.,0.));
#5830=DIRECTION('',(0.,-1.,0.));
#5831=DIRECTION('center_axis',(0.,0.,1.));
#5832=DIRECTION('ref_axis',(1.,0.,0.));
#5833=DIRECTION('center_axis',(0.,0.,1.));
#5834=DIRECTION('ref_axis',(1.,0.,0.));
#5835=DIRECTION('axis',(0.,0.,1.));
#5836=DIRECTION('refdir',(1.,0.,0.));
#5837=DIRECTION('center_axis',(0.,1.,0.));
#5838=DIRECTION('ref_axis',(-1.,0.,0.));
#5839=DIRECTION('',(-1.,0.,0.));
#5840=DIRECTION('',(0.,0.,1.));
#5841=DIRECTION('',(-1.,0.,0.));
#5842=DIRECTION('',(0.,0.,1.));
#5843=DIRECTION('center_axis',(1.,0.,0.));
#5844=DIRECTION('ref_axis',(0.,1.,0.));
#5845=DIRECTION('',(0.,1.,0.));
#5846=DIRECTION('',(0.,1.,0.));
#5847=DIRECTION('',(0.,0.,1.));
#5848=DIRECTION('center_axis',(0.,-1.,0.));
#5849=DIRECTION('ref_axis',(1.,0.,0.));
#5850=DIRECTION('',(1.,0.,0.));
#5851=DIRECTION('',(1.,0.,0.));
#5852=DIRECTION('',(0.,0.,1.));
#5853=DIRECTION('center_axis',(-1.,0.,0.));
#5854=DIRECTION('ref_axis',(0.,-1.,0.));
#5855=DIRECTION('',(0.,-1.,0.));
#5856=DIRECTION('',(0.,-1.,0.));
#5857=DIRECTION('center_axis',(0.,0.,1.));
#5858=DIRECTION('ref_axis',(1.,0.,0.));
#5859=DIRECTION('center_axis',(0.,0.,1.));
#5860=DIRECTION('ref_axis',(1.,0.,0.));
#5861=DIRECTION('axis',(0.,0.,1.));
#5862=DIRECTION('refdir',(1.,0.,0.));
#5863=DIRECTION('center_axis',(0.,1.,0.));
#5864=DIRECTION('ref_axis',(-1.,0.,0.));
#5865=DIRECTION('',(-1.,0.,0.));
#5866=DIRECTION('',(0.,0.,1.));
#5867=DIRECTION('',(-1.,0.,0.));
#5868=DIRECTION('',(0.,0.,1.));
#5869=DIRECTION('center_axis',(1.,0.,0.));
#5870=DIRECTION('ref_axis',(0.,1.,0.));
#5871=DIRECTION('',(0.,1.,0.));
#5872=DIRECTION('',(0.,1.,0.));
#5873=DIRECTION('',(0.,0.,1.));
#5874=DIRECTION('center_axis',(0.,-1.,0.));
#5875=DIRECTION('ref_axis',(1.,0.,0.));
#5876=DIRECTION('',(1.,0.,0.));
#5877=DIRECTION('',(1.,0.,0.));
#5878=DIRECTION('',(0.,0.,1.));
#5879=DIRECTION('center_axis',(-1.,0.,0.));
#5880=DIRECTION('ref_axis',(0.,-1.,0.));
#5881=DIRECTION('',(0.,-1.,0.));
#5882=DIRECTION('',(0.,-1.,0.));
#5883=DIRECTION('center_axis',(0.,0.,1.));
#5884=DIRECTION('ref_axis',(1.,0.,0.));
#5885=DIRECTION('center_axis',(0.,0.,1.));
#5886=DIRECTION('ref_axis',(1.,0.,0.));
#5887=DIRECTION('center_axis',(0.,0.,1.));
#5888=DIRECTION('ref_axis',(1.,0.,0.));
#5889=DIRECTION('center_axis',(0.,0.,1.));
#5890=DIRECTION('ref_axis',(1.,0.,0.));
#5891=DIRECTION('',(0.,0.,1.));
#5892=DIRECTION('center_axis',(0.,0.,-1.));
#5893=DIRECTION('ref_axis',(1.,0.,0.));
#5894=DIRECTION('center_axis',(0.,0.,1.));
#5895=DIRECTION('ref_axis',(1.,0.,0.));
#5896=DIRECTION('center_axis',(0.,0.,1.));
#5897=DIRECTION('ref_axis',(1.,0.,0.));
#5898=DIRECTION('',(0.,0.,1.));
#5899=DIRECTION('center_axis',(0.,0.,-1.));
#5900=DIRECTION('ref_axis',(1.,0.,0.));
#5901=DIRECTION('center_axis',(0.,0.,1.));
#5902=DIRECTION('ref_axis',(1.,0.,0.));
#5903=DIRECTION('center_axis',(0.,0.,1.));
#5904=DIRECTION('ref_axis',(1.,0.,0.));
#5905=DIRECTION('',(0.,0.,1.));
#5906=DIRECTION('center_axis',(0.,0.,-1.));
#5907=DIRECTION('ref_axis',(1.,0.,0.));
#5908=DIRECTION('center_axis',(0.,0.,1.));
#5909=DIRECTION('ref_axis',(1.,0.,0.));
#5910=DIRECTION('center_axis',(0.,0.,1.));
#5911=DIRECTION('ref_axis',(1.,0.,0.));
#5912=DIRECTION('',(0.,0.,1.));
#5913=DIRECTION('center_axis',(0.,0.,-1.));
#5914=DIRECTION('ref_axis',(1.,0.,0.));
#5915=DIRECTION('center_axis',(0.,1.,0.));
#5916=DIRECTION('ref_axis',(-1.,0.,0.));
#5917=DIRECTION('',(-1.,0.,0.));
#5918=DIRECTION('',(0.,0.,1.));
#5919=DIRECTION('',(-1.,0.,0.));
#5920=DIRECTION('',(0.,0.,1.));
#5921=DIRECTION('center_axis',(1.,0.,0.));
#5922=DIRECTION('ref_axis',(0.,1.,0.));
#5923=DIRECTION('',(0.,1.,0.));
#5924=DIRECTION('',(0.,1.,0.));
#5925=DIRECTION('',(0.,0.,1.));
#5926=DIRECTION('center_axis',(0.,-1.,0.));
#5927=DIRECTION('ref_axis',(1.,0.,0.));
#5928=DIRECTION('',(1.,0.,0.));
#5929=DIRECTION('',(1.,0.,0.));
#5930=DIRECTION('',(0.,0.,1.));
#5931=DIRECTION('center_axis',(-1.,0.,0.));
#5932=DIRECTION('ref_axis',(0.,-1.,0.));
#5933=DIRECTION('',(0.,-1.,0.));
#5934=DIRECTION('',(0.,-1.,0.));
#5935=DIRECTION('center_axis',(0.,0.,1.));
#5936=DIRECTION('ref_axis',(1.,0.,0.));
#5937=DIRECTION('center_axis',(0.,0.,1.));
#5938=DIRECTION('ref_axis',(1.,0.,0.));
#5939=DIRECTION('axis',(0.,0.,1.));
#5940=DIRECTION('refdir',(1.,0.,0.));
#5941=DIRECTION('center_axis',(0.,1.,0.));
#5942=DIRECTION('ref_axis',(1.,0.,0.));
#5943=DIRECTION('center_axis',(0.,1.,0.));
#5944=DIRECTION('ref_axis',(1.,0.,0.));
#5945=DIRECTION('',(0.,1.,0.));
#5946=DIRECTION('center_axis',(0.,-1.,0.));
#5947=DIRECTION('ref_axis',(1.,0.,0.));
#5948=DIRECTION('center_axis',(0.,1.,0.));
#5949=DIRECTION('ref_axis',(1.,0.,0.));
#5950=DIRECTION('center_axis',(0.,1.,0.));
#5951=DIRECTION('ref_axis',(1.,0.,0.));
#5952=DIRECTION('',(0.,1.,0.));
#5953=DIRECTION('center_axis',(0.,-1.,0.));
#5954=DIRECTION('ref_axis',(1.,0.,0.));
#5955=DIRECTION('center_axis',(0.,1.,0.));
#5956=DIRECTION('ref_axis',(1.,0.,0.));
#5957=DIRECTION('center_axis',(0.,1.,0.));
#5958=DIRECTION('ref_axis',(1.,0.,0.));
#5959=DIRECTION('',(0.,1.,0.));
#5960=DIRECTION('center_axis',(0.,-1.,0.));
#5961=DIRECTION('ref_axis',(1.,0.,0.));
#5962=DIRECTION('center_axis',(0.,1.,0.));
#5963=DIRECTION('ref_axis',(1.,0.,0.));
#5964=DIRECTION('center_axis',(0.,1.,0.));
#5965=DIRECTION('ref_axis',(1.,0.,0.));
#5966=DIRECTION('',(0.,1.,0.));
#5967=DIRECTION('center_axis',(0.,-1.,0.));
#5968=DIRECTION('ref_axis',(1.,0.,0.));
#5969=DIRECTION('center_axis',(0.,1.,0.));
#5970=DIRECTION('ref_axis',(-1.,0.,0.));
#5971=DIRECTION('',(-1.,0.,0.));
#5972=DIRECTION('',(0.,0.,1.));
#5973=DIRECTION('',(-1.,0.,0.));
#5974=DIRECTION('',(0.,0.,1.));
#5975=DIRECTION('center_axis',(1.,0.,0.));
#5976=DIRECTION('ref_axis',(0.,1.,0.));
#5977=DIRECTION('',(0.,1.,0.));
#5978=DIRECTION('',(0.,1.,0.));
#5979=DIRECTION('',(0.,0.,1.));
#5980=DIRECTION('center_axis',(0.,-1.,0.));
#5981=DIRECTION('ref_axis',(1.,0.,0.));
#5982=DIRECTION('',(1.,0.,0.));
#5983=DIRECTION('',(1.,0.,0.));
#5984=DIRECTION('',(0.,0.,1.));
#5985=DIRECTION('center_axis',(-1.,0.,0.));
#5986=DIRECTION('ref_axis',(0.,-1.,0.));
#5987=DIRECTION('',(0.,-1.,0.));
#5988=DIRECTION('',(0.,-1.,0.));
#5989=DIRECTION('center_axis',(0.,0.,1.));
#5990=DIRECTION('ref_axis',(1.,0.,0.));
#5991=DIRECTION('center_axis',(0.,0.,1.));
#5992=DIRECTION('ref_axis',(1.,0.,0.));
#5993=DIRECTION('axis',(0.,0.,1.));
#5994=DIRECTION('refdir',(1.,0.,0.));
#5995=DIRECTION('center_axis',(0.,0.,1.));
#5996=DIRECTION('ref_axis',(1.,0.,0.));
#5997=DIRECTION('center_axis',(0.,0.,1.));
#5998=DIRECTION('ref_axis',(1.,0.,0.));
#5999=DIRECTION('',(0.,0.,1.));
#6000=DIRECTION('center_axis',(0.,0.,-1.));
#6001=DIRECTION('ref_axis',(1.,0.,0.));
#6002=DIRECTION('center_axis',(0.,0.,1.));
#6003=DIRECTION('ref_axis',(1.,0.,0.));
#6004=DIRECTION('center_axis',(0.,0.,1.));
#6005=DIRECTION('ref_axis',(1.,0.,0.));
#6006=DIRECTION('',(0.,0.,1.));
#6007=DIRECTION('center_axis',(0.,0.,-1.));
#6008=DIRECTION('ref_axis',(1.,0.,0.));
#6009=DIRECTION('center_axis',(0.,0.,1.));
#6010=DIRECTION('ref_axis',(1.,0.,0.));
#6011=DIRECTION('center_axis',(0.,0.,1.));
#6012=DIRECTION('ref_axis',(1.,0.,0.));
#6013=DIRECTION('',(0.,0.,1.));
#6014=DIRECTION('center_axis',(0.,0.,-1.));
#6015=DIRECTION('ref_axis',(1.,0.,0.));
#6016=DIRECTION('center_axis',(0.,0.,1.));
#6017=DIRECTION('ref_axis',(1.,0.,0.));
#6018=DIRECTION('center_axis',(0.,0.,1.));
#6019=DIRECTION('ref_axis',(1.,0.,0.));
#6020=DIRECTION('',(0.,0.,1.));
#6021=DIRECTION('center_axis',(0.,0.,-1.));
#6022=DIRECTION('ref_axis',(1.,0.,0.));
#6023=DIRECTION('center_axis',(0.,0.,1.));
#6024=DIRECTION('ref_axis',(1.,0.,0.));
#6025=DIRECTION('center_axis',(0.,0.,1.));
#6026=DIRECTION('ref_axis',(1.,0.,0.));
#6027=DIRECTION('center_axis',(0.,0.,1.));
#6028=DIRECTION('ref_axis',(1.,0.,0.));
#6029=DIRECTION('center_axis',(0.,0.,1.));
#6030=DIRECTION('ref_axis',(1.,0.,0.));
#6031=DIRECTION('',(0.,0.,1.));
#6032=DIRECTION('center_axis',(0.,0.,1.));
#6033=DIRECTION('ref_axis',(1.,0.,0.));
#6034=DIRECTION('',(-1.,0.,0.));
#6035=DIRECTION('',(0.,-1.,0.));
#6036=DIRECTION('',(1.,0.,0.));
#6037=DIRECTION('center_axis',(0.,0.,1.));
#6038=DIRECTION('ref_axis',(1.,0.,0.));
#6039=DIRECTION('center_axis',(0.,1.,0.));
#6040=DIRECTION('ref_axis',(-1.,0.,0.));
#6041=DIRECTION('',(0.,0.,1.));
#6042=DIRECTION('',(-1.,0.,0.));
#6043=DIRECTION('',(0.,0.,1.));
#6044=DIRECTION('center_axis',(0.,-1.,0.));
#6045=DIRECTION('ref_axis',(1.,0.,0.));
#6046=DIRECTION('',(0.,0.,-1.));
#6047=DIRECTION('',(0.,0.,1.));
#6048=DIRECTION('',(1.,0.,0.));
#6049=DIRECTION('center_axis',(-1.,0.,0.));
#6050=DIRECTION('ref_axis',(0.,-1.,0.));
#6051=DIRECTION('',(0.,-1.,0.));
#6052=DIRECTION('center_axis',(0.,0.,1.));
#6053=DIRECTION('ref_axis',(1.,0.,0.));
#6054=DIRECTION('center_axis',(0.,0.,1.));
#6055=DIRECTION('ref_axis',(1.,0.,0.));
#6056=DIRECTION('center_axis',(0.,0.,1.));
#6057=DIRECTION('ref_axis',(1.,0.,0.));
#6058=DIRECTION('axis',(0.,0.,1.));
#6059=DIRECTION('refdir',(1.,0.,0.));
#6060=DIRECTION('center_axis',(0.,0.,1.));
#6061=DIRECTION('ref_axis',(1.,0.,0.));
#6062=DIRECTION('center_axis',(0.,0.,-1.));
#6063=DIRECTION('ref_axis',(1.,0.,0.));
#6064=DIRECTION('center_axis',(0.,0.,1.));
#6065=DIRECTION('ref_axis',(1.,0.,0.));
#6066=DIRECTION('center_axis',(0.,0.,1.));
#6067=DIRECTION('ref_axis',(1.,0.,0.));
#6068=DIRECTION('center_axis',(0.,0.,1.));
#6069=DIRECTION('ref_axis',(-1.,1.22464679914735E-16,0.));
#6070=DIRECTION('',(0.,0.,-1.));
#6071=DIRECTION('center_axis',(0.,0.,-1.));
#6072=DIRECTION('ref_axis',(1.,0.,0.));
#6073=DIRECTION('',(0.,0.,1.));
#6074=DIRECTION('center_axis',(0.,0.,1.));
#6075=DIRECTION('ref_axis',(1.,0.,0.));
#6076=DIRECTION('center_axis',(0.,0.,-1.));
#6077=DIRECTION('ref_axis',(1.,0.,0.));
#6078=DIRECTION('center_axis',(0.,0.,1.));
#6079=DIRECTION('ref_axis',(1.,0.,0.));
#6080=DIRECTION('center_axis',(0.,0.,1.));
#6081=DIRECTION('ref_axis',(1.,0.,0.));
#6082=DIRECTION('center_axis',(0.,0.,1.));
#6083=DIRECTION('ref_axis',(0.499999999999999,-0.866025403784439,0.));
#6084=DIRECTION('',(0.,0.,-1.));
#6085=DIRECTION('center_axis',(0.,0.,-1.));
#6086=DIRECTION('ref_axis',(1.,0.,0.));
#6087=DIRECTION('',(0.,0.,1.));
#6088=DIRECTION('center_axis',(0.,0.,1.));
#6089=DIRECTION('ref_axis',(1.,0.,0.));
#6090=DIRECTION('center_axis',(0.,0.,-1.));
#6091=DIRECTION('ref_axis',(1.,0.,0.));
#6092=DIRECTION('center_axis',(0.,0.,1.));
#6093=DIRECTION('ref_axis',(1.,0.,0.));
#6094=DIRECTION('center_axis',(0.,0.,1.));
#6095=DIRECTION('ref_axis',(1.,0.,0.));
#6096=DIRECTION('center_axis',(0.,0.,1.));
#6097=DIRECTION('ref_axis',(0.500000000000001,0.866025403784438,0.));
#6098=DIRECTION('',(0.,0.,-1.));
#6099=DIRECTION('center_axis',(0.,0.,-1.));
#6100=DIRECTION('ref_axis',(1.,0.,0.));
#6101=DIRECTION('',(0.,0.,1.));
#6102=DIRECTION('center_axis',(0.,0.,1.));
#6103=DIRECTION('ref_axis',(1.,0.,0.));
#6104=DIRECTION('center_axis',(0.,0.,1.));
#6105=DIRECTION('ref_axis',(1.,0.,0.));
#6106=DIRECTION('center_axis',(0.,0.,1.));
#6107=DIRECTION('ref_axis',(1.,0.,0.));
#6108=DIRECTION('',(0.,0.,-1.));
#6109=DIRECTION('center_axis',(0.,0.,1.));
#6110=DIRECTION('ref_axis',(1.,0.,0.));
#6111=DIRECTION('center_axis',(0.,0.,1.));
#6112=DIRECTION('ref_axis',(1.,0.,0.));
#6113=DIRECTION('center_axis',(0.,0.,1.));
#6114=DIRECTION('ref_axis',(1.,0.,0.));
#6115=DIRECTION('center_axis',(0.,0.,1.));
#6116=DIRECTION('ref_axis',(1.,0.,0.));
#6117=DIRECTION('center_axis',(0.,0.,1.));
#6118=DIRECTION('ref_axis',(1.,0.,0.));
#6119=DIRECTION('',(0.,0.,1.));
#6120=DIRECTION('center_axis',(0.,0.,1.));
#6121=DIRECTION('ref_axis',(1.,0.,0.));
#6122=DIRECTION('center_axis',(0.,0.,1.));
#6123=DIRECTION('ref_axis',(1.,0.,0.));
#6124=DIRECTION('',(0.,0.,1.));
#6125=DIRECTION('center_axis',(0.,0.,1.));
#6126=DIRECTION('ref_axis',(1.,0.,0.));
#6127=DIRECTION('center_axis',(0.,0.,1.));
#6128=DIRECTION('ref_axis',(1.,0.,0.));
#6129=DIRECTION('',(0.,0.,1.));
#6130=DIRECTION('center_axis',(0.,0.,1.));
#6131=DIRECTION('ref_axis',(1.,0.,0.));
#6132=DIRECTION('center_axis',(0.,0.,-1.));
#6133=DIRECTION('ref_axis',(1.,0.,0.));
#6134=DIRECTION('',(0.,0.,-1.));
#6135=DIRECTION('center_axis',(0.,0.,-1.));
#6136=DIRECTION('ref_axis',(1.,0.,0.));
#6137=DIRECTION('center_axis',(0.,0.,1.));
#6138=DIRECTION('ref_axis',(1.,0.,0.));
#6139=DIRECTION('center_axis',(0.,0.,1.));
#6140=DIRECTION('ref_axis',(1.,0.,0.));
#6141=DIRECTION('axis',(0.,0.,1.));
#6142=DIRECTION('refdir',(1.,0.,0.));
#6143=DIRECTION('center_axis',(0.,0.,1.));
#6144=DIRECTION('ref_axis',(1.,0.,0.));
#6145=DIRECTION('center_axis',(0.,0.,1.));
#6146=DIRECTION('ref_axis',(1.,0.,0.));
#6147=DIRECTION('',(0.,0.,1.));
#6148=DIRECTION('center_axis',(0.,0.,-1.));
#6149=DIRECTION('ref_axis',(1.,0.,0.));
#6150=DIRECTION('center_axis',(0.,0.,1.));
#6151=DIRECTION('ref_axis',(1.,0.,0.));
#6152=DIRECTION('center_axis',(0.,0.,1.));
#6153=DIRECTION('ref_axis',(1.,0.,0.));
#6154=DIRECTION('',(0.,0.,1.));
#6155=DIRECTION('center_axis',(0.,0.,-1.));
#6156=DIRECTION('ref_axis',(1.,0.,0.));
#6157=DIRECTION('center_axis',(0.,0.,1.));
#6158=DIRECTION('ref_axis',(1.,0.,0.));
#6159=DIRECTION('center_axis',(0.,0.,1.));
#6160=DIRECTION('ref_axis',(1.,0.,0.));
#6161=DIRECTION('',(0.,0.,1.));
#6162=DIRECTION('center_axis',(0.,0.,-1.));
#6163=DIRECTION('ref_axis',(1.,0.,0.));
#6164=DIRECTION('center_axis',(0.,0.,1.));
#6165=DIRECTION('ref_axis',(1.,0.,0.));
#6166=DIRECTION('center_axis',(0.,0.,1.));
#6167=DIRECTION('ref_axis',(1.,0.,0.));
#6168=DIRECTION('',(0.,0.,1.));
#6169=DIRECTION('center_axis',(0.,0.,1.));
#6170=DIRECTION('ref_axis',(1.,0.,0.));
#6171=DIRECTION('center_axis',(0.,0.,1.));
#6172=DIRECTION('ref_axis',(1.,0.,0.));
#6173=DIRECTION('center_axis',(0.,0.,-1.));
#6174=DIRECTION('ref_axis',(1.,0.,0.));
#6175=DIRECTION('center_axis',(0.,0.,1.));
#6176=DIRECTION('ref_axis',(1.,0.,0.));
#6177=DIRECTION('',(0.,0.,1.));
#6178=DIRECTION('center_axis',(0.,0.,-1.));
#6179=DIRECTION('ref_axis',(1.,0.,0.));
#6180=DIRECTION('center_axis',(0.,0.,1.));
#6181=DIRECTION('ref_axis',(1.,0.,0.));
#6182=DIRECTION('',(-1.,0.,0.));
#6183=DIRECTION('',(0.,-1.,0.));
#6184=DIRECTION('',(1.,0.,0.));
#6185=DIRECTION('center_axis',(0.,0.,1.));
#6186=DIRECTION('ref_axis',(1.,0.,0.));
#6187=DIRECTION('center_axis',(0.,1.,0.));
#6188=DIRECTION('ref_axis',(-1.,0.,0.));
#6189=DIRECTION('',(0.,0.,1.));
#6190=DIRECTION('',(-1.,0.,0.));
#6191=DIRECTION('',(0.,0.,1.));
#6192=DIRECTION('center_axis',(0.,-1.,0.));
#6193=DIRECTION('ref_axis',(1.,0.,0.));
#6194=DIRECTION('',(0.,0.,-1.));
#6195=DIRECTION('',(0.,0.,1.));
#6196=DIRECTION('',(1.,0.,0.));
#6197=DIRECTION('center_axis',(-1.,0.,0.));
#6198=DIRECTION('ref_axis',(0.,-1.,0.));
#6199=DIRECTION('',(0.,-1.,0.));
#6200=DIRECTION('center_axis',(0.,0.,1.));
#6201=DIRECTION('ref_axis',(1.,0.,0.));
#6202=DIRECTION('center_axis',(0.,0.,1.));
#6203=DIRECTION('ref_axis',(1.,0.,0.));
#6204=DIRECTION('center_axis',(0.,0.,1.));
#6205=DIRECTION('ref_axis',(1.,0.,0.));
#6206=DIRECTION('axis',(0.,0.,1.));
#6207=DIRECTION('refdir',(1.,0.,0.));
#6208=DIRECTION('center_axis',(0.,0.,1.));
#6209=DIRECTION('ref_axis',(-1.,1.22464679914735E-16,0.));
#6210=DIRECTION('',(0.,0.,-1.));
#6211=DIRECTION('center_axis',(0.,0.,1.));
#6212=DIRECTION('ref_axis',(1.,0.,0.));
#6213=DIRECTION('',(0.,0.,1.));
#6214=DIRECTION('center_axis',(0.,0.,1.));
#6215=DIRECTION('ref_axis',(1.,0.,0.));
#6216=DIRECTION('center_axis',(0.,0.,1.));
#6217=DIRECTION('ref_axis',(1.,0.,0.));
#6218=DIRECTION('center_axis',(0.,0.,1.));
#6219=DIRECTION('ref_axis',(1.,0.,0.));
#6220=DIRECTION('center_axis',(0.,0.,-1.));
#6221=DIRECTION('ref_axis',(1.,0.,0.));
#6222=DIRECTION('center_axis',(0.,0.,1.));
#6223=DIRECTION('ref_axis',(0.499999999999999,-0.866025403784439,0.));
#6224=DIRECTION('',(0.,0.,-1.));
#6225=DIRECTION('center_axis',(0.,0.,1.));
#6226=DIRECTION('ref_axis',(1.,0.,0.));
#6227=DIRECTION('',(0.,0.,1.));
#6228=DIRECTION('center_axis',(0.,0.,1.));
#6229=DIRECTION('ref_axis',(1.,0.,0.));
#6230=DIRECTION('center_axis',(0.,0.,1.));
#6231=DIRECTION('ref_axis',(1.,0.,0.));
#6232=DIRECTION('center_axis',(0.,0.,1.));
#6233=DIRECTION('ref_axis',(1.,0.,0.));
#6234=DIRECTION('center_axis',(0.,0.,-1.));
#6235=DIRECTION('ref_axis',(1.,0.,0.));
#6236=DIRECTION('center_axis',(0.,0.,1.));
#6237=DIRECTION('ref_axis',(0.500000000000001,0.866025403784438,0.));
#6238=DIRECTION('',(0.,0.,-1.));
#6239=DIRECTION('center_axis',(0.,0.,1.));
#6240=DIRECTION('ref_axis',(1.,0.,0.));
#6241=DIRECTION('',(0.,0.,1.));
#6242=DIRECTION('center_axis',(0.,0.,1.));
#6243=DIRECTION('ref_axis',(1.,0.,0.));
#6244=DIRECTION('center_axis',(0.,0.,1.));
#6245=DIRECTION('ref_axis',(1.,0.,0.));
#6246=DIRECTION('center_axis',(0.,0.,1.));
#6247=DIRECTION('ref_axis',(1.,0.,0.));
#6248=DIRECTION('center_axis',(0.,0.,-1.));
#6249=DIRECTION('ref_axis',(1.,0.,0.));
#6250=DIRECTION('center_axis',(0.,0.,1.));
#6251=DIRECTION('ref_axis',(1.,0.,0.));
#6252=DIRECTION('center_axis',(0.,0.,1.));
#6253=DIRECTION('ref_axis',(1.,0.,0.));
#6254=DIRECTION('center_axis',(0.,0.,1.));
#6255=DIRECTION('ref_axis',(1.,0.,0.));
#6256=DIRECTION('center_axis',(0.,0.,1.));
#6257=DIRECTION('ref_axis',(1.,0.,0.));
#6258=DIRECTION('center_axis',(0.,0.,1.));
#6259=DIRECTION('ref_axis',(1.,0.,0.));
#6260=DIRECTION('center_axis',(0.,0.,-1.));
#6261=DIRECTION('ref_axis',(1.,0.,0.));
#6262=DIRECTION('center_axis',(0.,0.,1.));
#6263=DIRECTION('ref_axis',(1.,0.,0.));
#6264=DIRECTION('',(0.,0.,1.));
#6265=DIRECTION('center_axis',(0.,0.,-1.));
#6266=DIRECTION('ref_axis',(1.,0.,0.));
#6267=DIRECTION('center_axis',(0.,0.,1.));
#6268=DIRECTION('ref_axis',(1.,0.,0.));
#6269=DIRECTION('',(0.,0.,1.));
#6270=DIRECTION('center_axis',(0.,0.,-1.));
#6271=DIRECTION('ref_axis',(1.,0.,0.));
#6272=DIRECTION('center_axis',(0.,0.,1.));
#6273=DIRECTION('ref_axis',(1.,0.,0.));
#6274=DIRECTION('',(0.,0.,1.));
#6275=DIRECTION('center_axis',(0.,0.,-1.));
#6276=DIRECTION('ref_axis',(1.,0.,0.));
#6277=DIRECTION('center_axis',(0.,0.,1.));
#6278=DIRECTION('ref_axis',(1.,0.,0.));
#6279=DIRECTION('center_axis',(0.,0.,-1.));
#6280=DIRECTION('ref_axis',(1.,0.,0.));
#6281=DIRECTION('',(0.,0.,-1.));
#6282=DIRECTION('center_axis',(0.,0.,1.));
#6283=DIRECTION('ref_axis',(1.,0.,0.));
#6284=DIRECTION('center_axis',(0.,0.,1.));
#6285=DIRECTION('ref_axis',(1.,0.,0.));
#6286=DIRECTION('',(0.,0.,-1.));
#6287=DIRECTION('center_axis',(0.,0.,1.));
#6288=DIRECTION('ref_axis',(1.,0.,0.));
#6289=DIRECTION('axis',(0.,0.,1.));
#6290=DIRECTION('refdir',(1.,0.,0.));
#6291=DIRECTION('center_axis',(0.,1.,0.));
#6292=DIRECTION('ref_axis',(1.,0.,0.));
#6293=DIRECTION('center_axis',(0.,1.,0.));
#6294=DIRECTION('ref_axis',(1.,0.,0.));
#6295=DIRECTION('',(0.,1.,0.));
#6296=DIRECTION('center_axis',(0.,-1.,0.));
#6297=DIRECTION('ref_axis',(1.,0.,0.));
#6298=DIRECTION('center_axis',(1.,0.,0.));
#6299=DIRECTION('ref_axis',(0.,0.,-1.));
#6300=DIRECTION('',(0.,0.,1.));
#6301=DIRECTION('',(0.,1.,0.));
#6302=DIRECTION('',(0.,0.,-1.));
#6303=DIRECTION('',(0.,1.,0.));
#6304=DIRECTION('center_axis',(0.,1.,0.));
#6305=DIRECTION('ref_axis',(0.,0.,1.));
#6306=DIRECTION('',(1.,0.,0.));
#6307=DIRECTION('',(-1.,0.,0.));
#6308=DIRECTION('',(0.,0.,1.));
#6309=DIRECTION('center_axis',(0.,0.,1.));
#6310=DIRECTION('ref_axis',(1.,0.,0.));
#6311=DIRECTION('',(-1.,0.,0.));
#6312=DIRECTION('',(0.,-1.,0.));
#6313=DIRECTION('',(1.,0.,0.));
#6314=DIRECTION('',(0.,1.,0.));
#6315=DIRECTION('',(-1.,0.,0.));
#6316=DIRECTION('',(0.,-1.,0.));
#6317=DIRECTION('',(1.,0.,0.));
#6318=DIRECTION('',(0.,1.,0.));
#6319=DIRECTION('center_axis',(-1.,0.,0.));
#6320=DIRECTION('ref_axis',(0.,0.,1.));
#6321=DIRECTION('',(0.,0.,-1.));
#6322=DIRECTION('',(0.,1.,0.));
#6323=DIRECTION('center_axis',(0.,1.,0.));
#6324=DIRECTION('ref_axis',(0.,0.,1.));
#6325=DIRECTION('',(0.,0.,1.));
#6326=DIRECTION('',(-1.,0.,0.));
#6327=DIRECTION('center_axis',(0.,1.,0.));
#6328=DIRECTION('ref_axis',(1.,0.,0.));
#6329=DIRECTION('',(1.,0.,0.));
#6330=DIRECTION('',(0.,0.,-1.));
#6331=DIRECTION('center_axis',(-1.,0.,0.));
#6332=DIRECTION('ref_axis',(0.,-1.,0.));
#6333=DIRECTION('',(0.,-1.,0.));
#6334=DIRECTION('',(0.,0.,1.));
#6335=DIRECTION('center_axis',(-1.,0.,0.));
#6336=DIRECTION('ref_axis',(0.,-1.,0.));
#6337=DIRECTION('',(0.,0.,1.));
#6338=DIRECTION('',(0.,-1.,0.));
#6339=DIRECTION('center_axis',(0.,1.,0.));
#6340=DIRECTION('ref_axis',(-1.,0.,0.));
#6341=DIRECTION('',(-1.,0.,0.));
#6342=DIRECTION('',(0.,0.,1.));
#6343=DIRECTION('center_axis',(1.,0.,0.));
#6344=DIRECTION('ref_axis',(0.,1.,0.));
#6345=DIRECTION('',(0.,1.,0.));
#6346=DIRECTION('',(0.,0.,1.));
#6347=DIRECTION('center_axis',(0.,-1.,0.));
#6348=DIRECTION('ref_axis',(1.,0.,0.));
#6349=DIRECTION('',(1.,0.,0.));
#6350=DIRECTION('center_axis',(0.,0.,1.));
#6351=DIRECTION('ref_axis',(1.,0.,0.));
#6352=DIRECTION('axis',(0.,0.,1.));
#6353=DIRECTION('refdir',(1.,0.,0.));
#6354=DIRECTION('center_axis',(6.12323399573677E-17,0.,1.));
#6355=DIRECTION('ref_axis',(1.,0.,0.));
#6356=DIRECTION('center_axis',(0.,-1.,0.));
#6357=DIRECTION('ref_axis',(-1.,0.,0.));
#6358=DIRECTION('axis',(0.,0.,1.));
#6359=DIRECTION('refdir',(1.,0.,0.));
#6360=DIRECTION('center_axis',(0.,1.,0.));
#6361=DIRECTION('ref_axis',(1.,0.,0.));
#6362=DIRECTION('center_axis',(0.,1.,0.));
#6363=DIRECTION('ref_axis',(1.,0.,0.));
#6364=DIRECTION('center_axis',(0.,-1.,0.));
#6365=DIRECTION('ref_axis',(1.,0.,0.));
#6366=DIRECTION('center_axis',(0.,1.,0.));
#6367=DIRECTION('ref_axis',(1.,0.,0.));
#6368=DIRECTION('center_axis',(0.,1.,0.));
#6369=DIRECTION('ref_axis',(1.,0.,0.));
#6370=DIRECTION('',(0.,-1.,0.));
#6371=DIRECTION('center_axis',(0.,1.,0.));
#6372=DIRECTION('ref_axis',(1.,0.,0.));
#6373=DIRECTION('',(0.,-1.,0.));
#6374=DIRECTION('center_axis',(0.,1.,0.));
#6375=DIRECTION('ref_axis',(1.,0.,0.));
#6376=DIRECTION('center_axis',(0.,1.,0.));
#6377=DIRECTION('ref_axis',(1.,0.,0.));
#6378=DIRECTION('center_axis',(0.,1.,0.));
#6379=DIRECTION('ref_axis',(1.,0.,0.));
#6380=DIRECTION('axis',(0.,0.,1.));
#6381=DIRECTION('refdir',(1.,0.,0.));
#6382=DIRECTION('center_axis',(0.,1.,0.));
#6383=DIRECTION('ref_axis',(1.,0.,0.));
#6384=DIRECTION('center_axis',(0.,1.,0.));
#6385=DIRECTION('ref_axis',(1.,0.,0.));
#6386=DIRECTION('center_axis',(0.,1.,0.));
#6387=DIRECTION('ref_axis',(1.,0.,0.));
#6388=DIRECTION('center_axis',(0.,1.,0.));
#6389=DIRECTION('ref_axis',(1.,0.,0.));
#6390=DIRECTION('',(0.,-1.,0.));
#6391=DIRECTION('center_axis',(0.,1.,0.));
#6392=DIRECTION('ref_axis',(1.,0.,0.));
#6393=DIRECTION('center_axis',(0.,1.,0.));
#6394=DIRECTION('ref_axis',(1.,0.,0.));
#6395=DIRECTION('center_axis',(0.,-1.,0.));
#6396=DIRECTION('ref_axis',(1.,0.,0.));
#6397=DIRECTION('center_axis',(0.,1.,0.));
#6398=DIRECTION('ref_axis',(1.,0.,0.));
#6399=DIRECTION('center_axis',(0.,-1.,0.));
#6400=DIRECTION('ref_axis',(1.,0.,0.));
#6401=DIRECTION('',(0.,-1.,0.));
#6402=DIRECTION('center_axis',(0.,1.,0.));
#6403=DIRECTION('ref_axis',(1.,0.,0.));
#6404=DIRECTION('center_axis',(0.,1.,0.));
#6405=DIRECTION('ref_axis',(1.,0.,0.));
#6406=DIRECTION('',(0.,-1.,0.));
#6407=DIRECTION('center_axis',(0.,1.,0.));
#6408=DIRECTION('ref_axis',(1.,0.,0.));
#6409=DIRECTION('axis',(0.,0.,1.));
#6410=DIRECTION('refdir',(1.,0.,0.));
#6411=DIRECTION('center_axis',(0.,1.,0.));
#6412=DIRECTION('ref_axis',(1.,0.,0.));
#6413=DIRECTION('center_axis',(0.,-1.,0.));
#6414=DIRECTION('ref_axis',(1.,0.,0.));
#6415=DIRECTION('',(0.,-1.,0.));
#6416=DIRECTION('center_axis',(0.,-1.,0.));
#6417=DIRECTION('ref_axis',(1.,0.,0.));
#6418=DIRECTION('center_axis',(0.,1.,0.));
#6419=DIRECTION('ref_axis',(1.,0.,0.));
#6420=DIRECTION('center_axis',(0.,1.,0.));
#6421=DIRECTION('ref_axis',(1.,0.,0.));
#6422=DIRECTION('',(0.,-1.,0.));
#6423=DIRECTION('center_axis',(0.,1.,0.));
#6424=DIRECTION('ref_axis',(1.,0.,0.));
#6425=DIRECTION('center_axis',(0.,1.,0.));
#6426=DIRECTION('ref_axis',(1.,0.,0.));
#6427=DIRECTION('center_axis',(0.,1.,0.));
#6428=DIRECTION('ref_axis',(1.,0.,0.));
#6429=DIRECTION('axis',(0.,0.,1.));
#6430=DIRECTION('refdir',(1.,0.,0.));
#6431=DIRECTION('center_axis',(-0.000133970394124395,-0.118176177591672,
0.992992634968536));
#6432=DIRECTION('ref_axis',(1.59438332031483E-5,-0.992992644005897,-0.118176176516135));
#6433=DIRECTION('center_axis',(0.000133970209996934,-0.118176177452328,
0.992992634985144));
#6434=DIRECTION('ref_axis',(0.970349186816215,0.240028974349624,0.0284349629466645));
#6435=DIRECTION('center_axis',(0.000133970209996934,-0.118176177452328,
0.992992634985144));
#6436=DIRECTION('ref_axis',(0.970349186816215,0.240028974349624,0.0284349629466645));
#6437=DIRECTION('center_axis',(-0.000133970394124395,-0.118176177591672,
0.992992634968536));
#6438=DIRECTION('ref_axis',(1.59438332031483E-5,-0.992992644005897,-0.118176176516135));
#6439=DIRECTION('axis',(0.,0.,1.));
#6440=DIRECTION('refdir',(1.,0.,0.));
#6441=DIRECTION('center_axis',(0.,1.,0.));
#6442=DIRECTION('ref_axis',(-1.,0.,0.));
#6443=DIRECTION('',(-1.,0.,0.));
#6444=DIRECTION('',(0.,0.,1.));
#6445=DIRECTION('',(-1.,0.,0.));
#6446=DIRECTION('',(0.,0.,1.));
#6447=DIRECTION('center_axis',(1.,0.,0.));
#6448=DIRECTION('ref_axis',(0.,1.,0.));
#6449=DIRECTION('',(0.,1.,0.));
#6450=DIRECTION('',(0.,1.,0.));
#6451=DIRECTION('',(0.,0.,1.));
#6452=DIRECTION('center_axis',(0.,-1.,0.));
#6453=DIRECTION('ref_axis',(1.,0.,0.));
#6454=DIRECTION('',(1.,0.,0.));
#6455=DIRECTION('',(1.,0.,0.));
#6456=DIRECTION('',(0.,0.,1.));
#6457=DIRECTION('center_axis',(-1.,0.,0.));
#6458=DIRECTION('ref_axis',(0.,-1.,0.));
#6459=DIRECTION('',(0.,-1.,0.));
#6460=DIRECTION('',(0.,-1.,0.));
#6461=DIRECTION('center_axis',(0.,0.,1.));
#6462=DIRECTION('ref_axis',(1.,0.,0.));
#6463=DIRECTION('center_axis',(0.,0.,1.));
#6464=DIRECTION('ref_axis',(1.,0.,0.));
#6465=DIRECTION('axis',(0.,0.,1.));
#6466=DIRECTION('refdir',(1.,0.,0.));
#6467=DIRECTION('center_axis',(0.,1.,0.));
#6468=DIRECTION('ref_axis',(-1.,0.,0.));
#6469=DIRECTION('',(-1.,0.,0.));
#6470=DIRECTION('',(0.,0.,1.));
#6471=DIRECTION('',(-1.,0.,0.));
#6472=DIRECTION('',(0.,0.,1.));
#6473=DIRECTION('center_axis',(1.,0.,0.));
#6474=DIRECTION('ref_axis',(0.,1.,0.));
#6475=DIRECTION('',(0.,1.,0.));
#6476=DIRECTION('',(0.,1.,0.));
#6477=DIRECTION('',(0.,0.,1.));
#6478=DIRECTION('center_axis',(0.,-1.,0.));
#6479=DIRECTION('ref_axis',(1.,0.,0.));
#6480=DIRECTION('',(1.,0.,0.));
#6481=DIRECTION('',(1.,0.,0.));
#6482=DIRECTION('',(0.,0.,1.));
#6483=DIRECTION('center_axis',(-1.,0.,0.));
#6484=DIRECTION('ref_axis',(0.,-1.,0.));
#6485=DIRECTION('',(0.,-1.,0.));
#6486=DIRECTION('',(0.,-1.,0.));
#6487=DIRECTION('center_axis',(0.,0.,1.));
#6488=DIRECTION('ref_axis',(1.,0.,0.));
#6489=DIRECTION('center_axis',(0.,0.,1.));
#6490=DIRECTION('ref_axis',(1.,0.,0.));
#6491=DIRECTION('axis',(0.,0.,1.));
#6492=DIRECTION('refdir',(1.,0.,0.));
#6493=DIRECTION('center_axis',(0.,1.,0.));
#6494=DIRECTION('ref_axis',(1.,0.,0.));
#6495=DIRECTION('center_axis',(0.,-1.,0.));
#6496=DIRECTION('ref_axis',(1.,0.,0.));
#6497=DIRECTION('',(0.,-1.,0.));
#6498=DIRECTION('center_axis',(0.,-1.,0.));
#6499=DIRECTION('ref_axis',(1.,0.,0.));
#6500=DIRECTION('center_axis',(0.,1.,0.));
#6501=DIRECTION('ref_axis',(1.,0.,0.));
#6502=DIRECTION('center_axis',(0.,1.,0.));
#6503=DIRECTION('ref_axis',(1.,0.,0.));
#6504=DIRECTION('',(0.,-1.,0.));
#6505=DIRECTION('center_axis',(0.,1.,0.));
#6506=DIRECTION('ref_axis',(1.,0.,0.));
#6507=DIRECTION('center_axis',(0.,1.,0.));
#6508=DIRECTION('ref_axis',(1.,0.,0.));
#6509=DIRECTION('center_axis',(0.,1.,0.));
#6510=DIRECTION('ref_axis',(1.,0.,0.));
#6511=DIRECTION('axis',(0.,0.,1.));
#6512=DIRECTION('refdir',(1.,0.,0.));
#6513=DIRECTION('center_axis',(0.866025403784439,0.,-0.5));
#6514=DIRECTION('ref_axis',(0.5,0.,0.866025403784439));
#6515=DIRECTION('',(-0.5,0.,-0.866025403784439));
#6516=DIRECTION('',(0.,-1.,0.));
#6517=DIRECTION('',(0.5,0.,0.866025403784439));
#6518=DIRECTION('',(0.,-1.,0.));
#6519=DIRECTION('center_axis',(1.92296268638356E-16,0.,-1.));
#6520=DIRECTION('ref_axis',(1.,0.,1.92296268638356E-16));
#6521=DIRECTION('',(-1.,0.,-1.92296268638356E-16));
#6522=DIRECTION('',(0.,-1.,0.));
#6523=DIRECTION('',(1.,0.,1.92296268638356E-16));
#6524=DIRECTION('center_axis',(-0.866025403784439,0.,-0.5));
#6525=DIRECTION('ref_axis',(0.5,0.,-0.866025403784439));
#6526=DIRECTION('',(-0.5,0.,0.866025403784438));
#6527=DIRECTION('',(0.,-1.,0.));
#6528=DIRECTION('',(0.5,0.,-0.866025403784438));
#6529=DIRECTION('center_axis',(-0.866025403784439,0.,0.5));
#6530=DIRECTION('ref_axis',(-0.5,0.,-0.866025403784439));
#6531=DIRECTION('',(0.5,0.,0.866025403784439));
#6532=DIRECTION('',(0.,-1.,0.));
#6533=DIRECTION('',(-0.5,0.,-0.866025403784439));
#6534=DIRECTION('center_axis',(-1.92296268638356E-16,0.,1.));
#6535=DIRECTION('ref_axis',(-1.,0.,-1.92296268638356E-16));
#6536=DIRECTION('',(1.,0.,1.92296268638356E-16));
#6537=DIRECTION('',(0.,-1.,0.));
#6538=DIRECTION('',(-1.,0.,-1.92296268638356E-16));
#6539=DIRECTION('center_axis',(0.866025403784439,0.,0.5));
#6540=DIRECTION('ref_axis',(-0.5,0.,0.866025403784439));
#6541=DIRECTION('',(0.5,0.,-0.866025403784439));
#6542=DIRECTION('',(-0.5,0.,0.866025403784439));
#6543=DIRECTION('center_axis',(0.,1.,0.));
#6544=DIRECTION('ref_axis',(1.,0.,0.));
#6545=DIRECTION('center_axis',(0.,-1.,0.));
#6546=DIRECTION('ref_axis',(0.,0.,-1.));
#6547=DIRECTION('center_axis',(0.,1.,0.));
#6548=DIRECTION('ref_axis',(1.,0.,0.));
#6549=DIRECTION('center_axis',(0.,1.,0.));
#6550=DIRECTION('ref_axis',(1.,0.,0.));
#6551=DIRECTION('center_axis',(0.,1.,0.));
#6552=DIRECTION('ref_axis',(0.,0.,1.));
#6553=DIRECTION('center_axis',(0.,-1.,0.));
#6554=DIRECTION('ref_axis',(1.,0.,0.));
#6555=DIRECTION('center_axis',(0.,-1.,0.));
#6556=DIRECTION('ref_axis',(1.,0.,0.));
#6557=DIRECTION('center_axis',(0.,-1.,0.));
#6558=DIRECTION('ref_axis',(1.,0.,0.));
#6559=DIRECTION('',(0.707106781186548,0.707106781186547,8.65956056235494E-17));
#6560=DIRECTION('center_axis',(0.,-1.,0.));
#6561=DIRECTION('ref_axis',(1.,0.,0.));
#6562=DIRECTION('center_axis',(0.,-1.,0.));
#6563=DIRECTION('ref_axis',(1.,0.,0.));
#6564=DIRECTION('',(0.,1.,0.));
#6565=DIRECTION('center_axis',(0.,1.,0.));
#6566=DIRECTION('ref_axis',(1.,0.,0.));
#6567=DIRECTION('center_axis',(0.,-1.,0.));
#6568=DIRECTION('ref_axis',(1.,0.,0.));
#6569=DIRECTION('',(-0.707106781186547,0.707106781186548,-8.65956056235493E-17));
#6570=DIRECTION('center_axis',(0.,-1.,0.));
#6571=DIRECTION('ref_axis',(0.,0.,-1.));
#6572=DIRECTION('center_axis',(0.,-1.,0.));
#6573=DIRECTION('ref_axis',(1.,0.,0.));
#6574=DIRECTION('center_axis',(0.,1.,0.));
#6575=DIRECTION('ref_axis',(1.,0.,0.));
#6576=DIRECTION('center_axis',(0.,1.,0.));
#6577=DIRECTION('ref_axis',(1.,0.,0.));
#6578=DIRECTION('',(-0.447213595499958,0.894427190999916,-5.47678698264203E-17));
#6579=DIRECTION('center_axis',(0.,-1.,0.));
#6580=DIRECTION('ref_axis',(1.,0.,0.));
#6581=DIRECTION('',(0.,1.,0.));
#6582=DIRECTION('axis',(0.,0.,1.));
#6583=DIRECTION('refdir',(1.,0.,0.));
#6584=DIRECTION('axis',(0.,0.,1.));
#6585=DIRECTION('refdir',(1.,0.,0.));
#6586=DIRECTION('center_axis',(0.,-1.,0.));
#6587=DIRECTION('ref_axis',(0.,0.,-1.));
#6588=DIRECTION('center_axis',(0.,-1.,0.));
#6589=DIRECTION('ref_axis',(1.,0.,0.));
#6590=DIRECTION('center_axis',(0.,-1.,0.));
#6591=DIRECTION('ref_axis',(1.,0.,0.));
#6592=DIRECTION('center_axis',(1.,0.,1.22464679914735E-16));
#6593=DIRECTION('ref_axis',(-1.22464679914735E-16,0.,1.));
#6594=DIRECTION('center_axis',(0.,1.,0.));
#6595=DIRECTION('ref_axis',(1.,0.,0.));
#6596=DIRECTION('center_axis',(0.,1.,0.));
#6597=DIRECTION('ref_axis',(1.,0.,0.));
#6598=DIRECTION('center_axis',(0.,-1.,0.));
#6599=DIRECTION('ref_axis',(1.,0.,0.));
#6600=DIRECTION('',(0.,1.,0.));
#6601=DIRECTION('center_axis',(0.,-1.,0.));
#6602=DIRECTION('ref_axis',(1.,0.,0.));
#6603=DIRECTION('center_axis',(0.,-1.,0.));
#6604=DIRECTION('ref_axis',(1.,0.,0.));
#6605=DIRECTION('center_axis',(0.,-1.,0.));
#6606=DIRECTION('ref_axis',(1.,0.,0.));
#6607=DIRECTION('',(0.,1.,0.));
#6608=DIRECTION('center_axis',(0.,-1.,0.));
#6609=DIRECTION('ref_axis',(1.,0.,0.));
#6610=DIRECTION('center_axis',(0.,1.,0.));
#6611=DIRECTION('ref_axis',(1.,0.,0.));
#6612=DIRECTION('',(-0.707106781186547,0.707106781186548,-8.65956056235493E-17));
#6613=DIRECTION('center_axis',(0.,-1.,0.));
#6614=DIRECTION('ref_axis',(1.,0.,0.));
#6615=DIRECTION('center_axis',(0.,1.,0.));
#6616=DIRECTION('ref_axis',(0.,0.,1.));
#6617=DIRECTION('center_axis',(0.,-1.,0.));
#6618=DIRECTION('ref_axis',(1.,0.,0.));
#6619=DIRECTION('center_axis',(0.,-1.,0.));
#6620=DIRECTION('ref_axis',(1.,0.,0.));
#6621=DIRECTION('',(0.,1.,0.));
#6622=DIRECTION('center_axis',(0.,-1.,0.));
#6623=DIRECTION('ref_axis',(0.,0.,-1.));
#6624=DIRECTION('center_axis',(0.,-1.,0.));
#6625=DIRECTION('ref_axis',(1.,0.,0.));
#6626=DIRECTION('center_axis',(0.,-1.,0.));
#6627=DIRECTION('ref_axis',(1.,0.,0.));
#6628=DIRECTION('',(0.707106781186547,0.707106781186548,8.65956056235493E-17));
#6629=DIRECTION('axis',(0.,0.,1.));
#6630=DIRECTION('refdir',(1.,0.,0.));
#6631=DIRECTION('center_axis',(0.,-1.,0.));
#6632=DIRECTION('ref_axis',(0.,0.,-1.));
#6633=DIRECTION('center_axis',(0.,-1.,0.));
#6634=DIRECTION('ref_axis',(1.,0.,0.));
#6635=DIRECTION('center_axis',(0.,-1.,0.));
#6636=DIRECTION('ref_axis',(1.,0.,0.));
#6637=DIRECTION('center_axis',(1.,0.,1.22464679914735E-16));
#6638=DIRECTION('ref_axis',(-1.22464679914735E-16,0.,1.));
#6639=DIRECTION('center_axis',(0.,1.,0.));
#6640=DIRECTION('ref_axis',(1.,0.,0.));
#6641=DIRECTION('center_axis',(0.,1.,0.));
#6642=DIRECTION('ref_axis',(1.,0.,0.));
#6643=DIRECTION('center_axis',(0.,-1.,0.));
#6644=DIRECTION('ref_axis',(1.,0.,0.));
#6645=DIRECTION('center_axis',(0.,-1.,0.));
#6646=DIRECTION('ref_axis',(1.,0.,0.));
#6647=DIRECTION('',(0.,1.,0.));
#6648=DIRECTION('center_axis',(0.,1.,0.));
#6649=DIRECTION('ref_axis',(0.,0.,1.));
#6650=DIRECTION('center_axis',(0.,-1.,0.));
#6651=DIRECTION('ref_axis',(1.,0.,0.));
#6652=DIRECTION('center_axis',(0.,-1.,0.));
#6653=DIRECTION('ref_axis',(1.,0.,0.));
#6654=DIRECTION('center_axis',(0.,-1.,0.));
#6655=DIRECTION('ref_axis',(1.,0.,0.));
#6656=DIRECTION('center_axis',(0.,-1.,0.));
#6657=DIRECTION('ref_axis',(1.,0.,0.));
#6658=DIRECTION('',(0.707106781186548,0.707106781186547,8.65956056235494E-17));
#6659=DIRECTION('center_axis',(0.,-1.,0.));
#6660=DIRECTION('ref_axis',(1.,0.,0.));
#6661=DIRECTION('center_axis',(0.,-1.,0.));
#6662=DIRECTION('ref_axis',(1.,0.,0.));
#6663=DIRECTION('',(0.,1.,0.));
#6664=DIRECTION('center_axis',(0.,1.,0.));
#6665=DIRECTION('ref_axis',(1.,0.,0.));
#6666=DIRECTION('center_axis',(0.,-1.,0.));
#6667=DIRECTION('ref_axis',(1.,0.,0.));
#6668=DIRECTION('',(-0.707106781186548,0.707106781186547,-8.65956056235494E-17));
#6669=DIRECTION('center_axis',(0.,-1.,0.));
#6670=DIRECTION('ref_axis',(0.,0.,-1.));
#6671=DIRECTION('center_axis',(0.,-1.,0.));
#6672=DIRECTION('ref_axis',(1.,0.,0.));
#6673=DIRECTION('',(0.,1.,0.));
#6674=DIRECTION('axis',(0.,0.,1.));
#6675=DIRECTION('refdir',(1.,0.,0.));
#6676=DIRECTION('center_axis',(0.,0.,1.));
#6677=DIRECTION('ref_axis',(1.,0.,0.));
#6678=DIRECTION('center_axis',(1.22464679914735E-16,-1.,0.));
#6679=DIRECTION('ref_axis',(-1.,-1.22464679914735E-16,0.));
#6680=DIRECTION('center_axis',(0.707106781186548,0.,0.707106781186548));
#6681=DIRECTION('ref_axis',(0.707106781186548,0.,-0.707106781186548));
#6682=DIRECTION('center_axis',(8.65956056235494E-17,-1.,-8.65956056235493E-17));
#6683=DIRECTION('ref_axis',(-0.707106781186547,-1.22464679914735E-16,0.707106781186547));
#6684=DIRECTION('center_axis',(1.,0.,0.));
#6685=DIRECTION('ref_axis',(6.12323399573676E-17,0.,-1.));
#6686=DIRECTION('center_axis',(7.49879891330929E-33,-1.,-1.22464679914735E-16));
#6687=DIRECTION('ref_axis',(-6.12323399573676E-17,-1.22464679914735E-16,
1.));
#6688=DIRECTION('center_axis',(0.707106781186548,0.,-0.707106781186548));
#6689=DIRECTION('ref_axis',(-0.707106781186548,0.,-0.707106781186548));
#6690=DIRECTION('center_axis',(-8.65956056235493E-17,-1.,-8.65956056235494E-17));
#6691=DIRECTION('ref_axis',(0.707106781186547,-1.22464679914735E-16,0.707106781186547));
#6692=DIRECTION('center_axis',(0.,0.,-1.));
#6693=DIRECTION('ref_axis',(-1.,0.,-1.22464679914735E-16));
#6694=DIRECTION('center_axis',(-1.22464679914735E-16,-1.,-1.49975978266186E-32));
#6695=DIRECTION('ref_axis',(1.,-1.22464679914735E-16,1.22464679914735E-16));
#6696=DIRECTION('center_axis',(-0.707106781186547,0.,-0.707106781186548));
#6697=DIRECTION('ref_axis',(-0.707106781186548,0.,0.707106781186547));
#6698=DIRECTION('center_axis',(-8.65956056235493E-17,-1.,8.65956056235493E-17));
#6699=DIRECTION('ref_axis',(0.707106781186548,-1.22464679914735E-16,-0.707106781186547));
#6700=DIRECTION('center_axis',(-1.,0.,0.));
#6701=DIRECTION('ref_axis',(-1.83697019872103E-16,0.,1.));
#6702=DIRECTION('center_axis',(-2.24963967399279E-32,-1.,1.22464679914735E-16));
#6703=DIRECTION('ref_axis',(1.83697019872103E-16,-1.22464679914735E-16,
-1.));
#6704=DIRECTION('center_axis',(-0.707106781186548,0.,0.707106781186548));
#6705=DIRECTION('ref_axis',(0.707106781186547,0.,0.707106781186548));
#6706=DIRECTION('center_axis',(8.65956056235493E-17,-1.,8.65956056235493E-17));
#6707=DIRECTION('ref_axis',(-0.707106781186547,-1.22464679914735E-16,-0.707106781186548));
#6708=DIRECTION('axis',(0.,0.,1.));
#6709=DIRECTION('refdir',(1.,0.,0.));
#6710=DIRECTION('center_axis',(0.,0.,1.));
#6711=DIRECTION('ref_axis',(1.,0.,0.));
#6712=DIRECTION('center_axis',(0.,-1.,0.));
#6713=DIRECTION('ref_axis',(0.,0.,-1.));
#6714=DIRECTION('center_axis',(0.,-1.,0.));
#6715=DIRECTION('ref_axis',(0.,0.,-1.));
#6716=DIRECTION('center_axis',(0.,1.,0.));
#6717=DIRECTION('ref_axis',(1.,0.,0.));
#6718=DIRECTION('center_axis',(0.,1.,0.));
#6719=DIRECTION('ref_axis',(1.,0.,0.));
#6720=DIRECTION('center_axis',(0.,1.,0.));
#6721=DIRECTION('ref_axis',(1.,0.,0.));
#6722=DIRECTION('center_axis',(0.,1.,0.));
#6723=DIRECTION('ref_axis',(1.,0.,0.));
#6724=DIRECTION('',(0.,-1.,0.));
#6725=DIRECTION('center_axis',(0.,-1.,0.));
#6726=DIRECTION('ref_axis',(1.,0.,0.));
#6727=DIRECTION('center_axis',(0.,1.,0.));
#6728=DIRECTION('ref_axis',(1.,0.,0.));
#6729=DIRECTION('center_axis',(0.,1.,0.));
#6730=DIRECTION('ref_axis',(1.,0.,0.));
#6731=DIRECTION('center_axis',(0.,1.,0.));
#6732=DIRECTION('ref_axis',(1.,0.,0.));
#6733=DIRECTION('center_axis',(0.,1.,0.));
#6734=DIRECTION('ref_axis',(1.,0.,0.));
#6735=DIRECTION('center_axis',(0.,1.,0.));
#6736=DIRECTION('ref_axis',(1.,0.,0.));
#6737=DIRECTION('center_axis',(0.,1.,0.));
#6738=DIRECTION('ref_axis',(1.,0.,0.));
#6739=DIRECTION('center_axis',(0.,-1.,0.));
#6740=DIRECTION('ref_axis',(1.,0.,0.));
#6741=DIRECTION('center_axis',(0.,-1.,0.));
#6742=DIRECTION('ref_axis',(0.,0.,-1.));
#6743=DIRECTION('center_axis',(6.12323399573677E-17,0.,1.));
#6744=DIRECTION('ref_axis',(1.,0.,0.));
#6745=DIRECTION('center_axis',(0.,-1.,0.));
#6746=DIRECTION('ref_axis',(0.,0.,-1.));
#6747=DIRECTION('center_axis',(0.,1.,0.));
#6748=DIRECTION('ref_axis',(1.,0.,0.));
#6749=DIRECTION('center_axis',(0.,-1.,0.));
#6750=DIRECTION('ref_axis',(1.,0.,0.));
#6751=DIRECTION('center_axis',(0.,-1.,0.));
#6752=DIRECTION('ref_axis',(0.,0.,-1.));
#6753=DIRECTION('center_axis',(0.,0.,1.));
#6754=DIRECTION('ref_axis',(1.,0.,0.));
#6755=DIRECTION('center_axis',(0.,-1.,0.));
#6756=DIRECTION('ref_axis',(0.,0.,-1.));
#6757=DIRECTION('center_axis',(0.,1.,0.));
#6758=DIRECTION('ref_axis',(1.,0.,0.));
#6759=DIRECTION('center_axis',(0.,-1.,0.));
#6760=DIRECTION('ref_axis',(1.,0.,0.));
#6761=DIRECTION('center_axis',(0.,-1.,0.));
#6762=DIRECTION('ref_axis',(0.,0.,-1.));
#6763=DIRECTION('center_axis',(0.,0.,1.));
#6764=DIRECTION('ref_axis',(1.,0.,0.));
#6765=DIRECTION('center_axis',(0.,-1.,0.));
#6766=DIRECTION('ref_axis',(0.,0.,-1.));
#6767=DIRECTION('center_axis',(0.,1.,0.));
#6768=DIRECTION('ref_axis',(1.,0.,0.));
#6769=DIRECTION('center_axis',(0.,-1.,0.));
#6770=DIRECTION('ref_axis',(1.,0.,0.));
#6771=DIRECTION('center_axis',(0.,-1.,0.));
#6772=DIRECTION('ref_axis',(0.,0.,-1.));
#6773=DIRECTION('center_axis',(0.,0.,1.));
#6774=DIRECTION('ref_axis',(1.,0.,0.));
#6775=DIRECTION('center_axis',(0.,-1.,0.));
#6776=DIRECTION('ref_axis',(0.,0.,-1.));
#6777=DIRECTION('center_axis',(0.,1.,0.));
#6778=DIRECTION('ref_axis',(1.,0.,0.));
#6779=DIRECTION('center_axis',(0.,-1.,0.));
#6780=DIRECTION('ref_axis',(1.,0.,0.));
#6781=DIRECTION('center_axis',(0.,-1.,0.));
#6782=DIRECTION('ref_axis',(0.,0.,-1.));
#6783=DIRECTION('center_axis',(6.12323399573676E-17,0.,1.));
#6784=DIRECTION('ref_axis',(1.,0.,0.));
#6785=DIRECTION('center_axis',(0.,-1.,0.));
#6786=DIRECTION('ref_axis',(0.,0.,-1.));
#6787=DIRECTION('center_axis',(0.,1.,0.));
#6788=DIRECTION('ref_axis',(1.,0.,0.));
#6789=DIRECTION('center_axis',(0.,-1.,0.));
#6790=DIRECTION('ref_axis',(1.,0.,0.));
#6791=DIRECTION('center_axis',(0.,-1.,0.));
#6792=DIRECTION('ref_axis',(0.,0.,-1.));
#6793=DIRECTION('center_axis',(0.,0.,1.));
#6794=DIRECTION('ref_axis',(1.,0.,0.));
#6795=DIRECTION('center_axis',(0.,-1.,0.));
#6796=DIRECTION('ref_axis',(0.,0.,-1.));
#6797=DIRECTION('center_axis',(0.,1.,0.));
#6798=DIRECTION('ref_axis',(1.,0.,0.));
#6799=DIRECTION('center_axis',(0.,1.,0.));
#6800=DIRECTION('ref_axis',(1.,0.,0.));
#6801=DIRECTION('',(0.,1.,0.));
#6802=DIRECTION('center_axis',(0.,-1.,0.));
#6803=DIRECTION('ref_axis',(1.,0.,0.));
#6804=DIRECTION('center_axis',(0.,-1.,0.));
#6805=DIRECTION('ref_axis',(1.,0.,0.));
#6806=DIRECTION('center_axis',(0.,1.,0.));
#6807=DIRECTION('ref_axis',(1.,0.,0.));
#6808=DIRECTION('center_axis',(0.,-1.,0.));
#6809=DIRECTION('ref_axis',(0.,0.,-1.));
#6810=DIRECTION('center_axis',(0.,0.,1.));
#6811=DIRECTION('ref_axis',(1.,0.,0.));
#6812=DIRECTION('center_axis',(0.,-1.,0.));
#6813=DIRECTION('ref_axis',(0.,0.,-1.));
#6814=DIRECTION('center_axis',(0.,-1.,0.));
#6815=DIRECTION('ref_axis',(-1.,0.,0.));
#6816=DIRECTION('center_axis',(0.,1.,0.));
#6817=DIRECTION('ref_axis',(1.,0.,0.));
#6818=DIRECTION('axis',(0.,0.,1.));
#6819=DIRECTION('refdir',(1.,0.,0.));
#6820=DIRECTION('center_axis',(0.,1.,0.));
#6821=DIRECTION('ref_axis',(0.,0.,1.));
#6822=DIRECTION('center_axis',(0.,-1.,0.));
#6823=DIRECTION('ref_axis',(1.,0.,0.));
#6824=DIRECTION('center_axis',(0.,-1.,0.));
#6825=DIRECTION('ref_axis',(1.,0.,0.));
#6826=DIRECTION('center_axis',(0.,-1.,0.));
#6827=DIRECTION('ref_axis',(1.,0.,0.));
#6828=DIRECTION('center_axis',(0.,-1.,0.));
#6829=DIRECTION('ref_axis',(1.,0.,0.));
#6830=DIRECTION('',(0.,1.,0.));
#6831=DIRECTION('center_axis',(0.,-1.,0.));
#6832=DIRECTION('ref_axis',(0.,0.,-1.));
#6833=DIRECTION('center_axis',(0.,-1.,0.));
#6834=DIRECTION('ref_axis',(1.,0.,0.));
#6835=DIRECTION('center_axis',(0.,-1.,0.));
#6836=DIRECTION('ref_axis',(1.,0.,0.));
#6837=DIRECTION('',(0.,1.,0.));
#6838=DIRECTION('center_axis',(0.,1.,0.));
#6839=DIRECTION('ref_axis',(0.,0.,1.));
#6840=DIRECTION('center_axis',(0.,-1.,0.));
#6841=DIRECTION('ref_axis',(1.,0.,0.));
#6842=DIRECTION('center_axis',(0.,-1.,0.));
#6843=DIRECTION('ref_axis',(1.,0.,0.));
#6844=DIRECTION('center_axis',(0.,-1.,0.));
#6845=DIRECTION('ref_axis',(1.,0.,0.));
#6846=DIRECTION('center_axis',(0.,-1.,0.));
#6847=DIRECTION('ref_axis',(1.,0.,0.));
#6848=DIRECTION('',(0.,1.,0.));
#6849=DIRECTION('center_axis',(0.,-1.,0.));
#6850=DIRECTION('ref_axis',(0.,0.,-1.));
#6851=DIRECTION('center_axis',(0.,-1.,0.));
#6852=DIRECTION('ref_axis',(1.,0.,0.));
#6853=DIRECTION('center_axis',(0.,-1.,0.));
#6854=DIRECTION('ref_axis',(1.,0.,0.));
#6855=DIRECTION('',(0.,1.,0.));
#6856=DIRECTION('',(0.,0.,1.));
#6857=DIRECTION('',(1.,0.,0.));
#6858=DIRECTION('',(0.,0.,1.));
#6859=DIRECTION('',(1.,0.,0.));
#6860=DIRECTION('',(0.,0.,1.));
#6861=DIRECTION('',(1.,0.,0.));
#6862=DIRECTION('',(0.,0.,1.));
#6863=DIRECTION('',(1.,0.,0.));
#6864=DIRECTION('',(0.,0.,1.));
#6865=DIRECTION('',(1.,0.,0.));
#6866=DIRECTION('axis',(0.,0.,1.));
#6867=DIRECTION('refdir',(1.,0.,0.));
#6868=DIRECTION('center_axis',(0.866025403784439,0.,-0.5));
#6869=DIRECTION('ref_axis',(0.5,0.,0.866025403784439));
#6870=DIRECTION('',(-0.5,0.,-0.866025403784439));
#6871=DIRECTION('',(0.,-1.,0.));
#6872=DIRECTION('',(0.5,0.,0.866025403784439));
#6873=DIRECTION('',(0.,-1.,0.));
#6874=DIRECTION('center_axis',(1.60246890531964E-16,0.,-1.));
#6875=DIRECTION('ref_axis',(1.,0.,1.60246890531964E-16));
#6876=DIRECTION('',(-1.,0.,-1.60246890531964E-16));
#6877=DIRECTION('',(0.,-1.,0.));
#6878=DIRECTION('',(1.,0.,1.60246890531964E-16));
#6879=DIRECTION('center_axis',(-0.866025403784439,0.,-0.5));
#6880=DIRECTION('ref_axis',(0.5,0.,-0.866025403784439));
#6881=DIRECTION('',(-0.5,0.,0.866025403784439));
#6882=DIRECTION('',(0.,-1.,0.));
#6883=DIRECTION('',(0.5,0.,-0.866025403784439));
#6884=DIRECTION('center_axis',(-0.866025403784439,0.,0.5));
#6885=DIRECTION('ref_axis',(-0.5,0.,-0.866025403784439));
#6886=DIRECTION('',(0.5,0.,0.866025403784439));
#6887=DIRECTION('',(0.,-1.,0.));
#6888=DIRECTION('',(-0.5,0.,-0.866025403784439));
#6889=DIRECTION('center_axis',(-1.60246890531964E-16,0.,1.));
#6890=DIRECTION('ref_axis',(-1.,0.,-1.60246890531964E-16));
#6891=DIRECTION('',(1.,0.,1.60246890531964E-16));
#6892=DIRECTION('',(0.,-1.,0.));
#6893=DIRECTION('',(-1.,0.,-1.60246890531964E-16));
#6894=DIRECTION('center_axis',(0.866025403784439,0.,0.5));
#6895=DIRECTION('ref_axis',(-0.5,0.,0.866025403784439));
#6896=DIRECTION('',(0.5,0.,-0.866025403784439));
#6897=DIRECTION('',(-0.5,0.,0.866025403784439));
#6898=DIRECTION('center_axis',(0.,1.,0.));
#6899=DIRECTION('ref_axis',(1.,0.,0.));
#6900=DIRECTION('center_axis',(0.,-1.,0.));
#6901=DIRECTION('ref_axis',(0.,0.,-1.));
#6902=DIRECTION('center_axis',(0.,1.,0.));
#6903=DIRECTION('ref_axis',(1.,0.,0.));
#6904=DIRECTION('center_axis',(0.,1.,0.));
#6905=DIRECTION('ref_axis',(1.,0.,0.));
#6906=DIRECTION('center_axis',(0.,1.,0.));
#6907=DIRECTION('ref_axis',(0.,0.,1.));
#6908=DIRECTION('center_axis',(0.,-1.,0.));
#6909=DIRECTION('ref_axis',(1.,0.,0.));
#6910=DIRECTION('center_axis',(0.,-1.,0.));
#6911=DIRECTION('ref_axis',(1.,0.,0.));
#6912=DIRECTION('center_axis',(0.,-1.,0.));
#6913=DIRECTION('ref_axis',(1.,0.,0.));
#6914=DIRECTION('',(0.707106781186547,0.707106781186548,8.65956056235493E-17));
#6915=DIRECTION('center_axis',(0.,-1.,0.));
#6916=DIRECTION('ref_axis',(1.,0.,0.));
#6917=DIRECTION('center_axis',(0.,-1.,0.));
#6918=DIRECTION('ref_axis',(1.,0.,0.));
#6919=DIRECTION('',(0.,1.,0.));
#6920=DIRECTION('center_axis',(0.,1.,0.));
#6921=DIRECTION('ref_axis',(1.,0.,0.));
#6922=DIRECTION('center_axis',(0.,-1.,0.));
#6923=DIRECTION('ref_axis',(1.,0.,0.));
#6924=DIRECTION('',(-0.707106781186547,0.707106781186548,-8.65956056235493E-17));
#6925=DIRECTION('center_axis',(0.,-1.,0.));
#6926=DIRECTION('ref_axis',(0.,0.,-1.));
#6927=DIRECTION('center_axis',(0.,-1.,0.));
#6928=DIRECTION('ref_axis',(1.,0.,0.));
#6929=DIRECTION('center_axis',(0.,1.,0.));
#6930=DIRECTION('ref_axis',(1.,0.,0.));
#6931=DIRECTION('center_axis',(0.,1.,0.));
#6932=DIRECTION('ref_axis',(1.,0.,0.));
#6933=DIRECTION('',(-0.447213595499958,0.894427190999916,-5.47678698264203E-17));
#6934=DIRECTION('center_axis',(0.,-1.,0.));
#6935=DIRECTION('ref_axis',(1.,0.,0.));
#6936=DIRECTION('',(0.,1.,0.));
#6937=DIRECTION('',(0.,0.,1.));
#6938=DIRECTION('',(1.,0.,0.));
#6939=DIRECTION('',(0.,0.,1.));
#6940=DIRECTION('',(1.,0.,0.));
#6941=DIRECTION('',(0.,0.,1.));
#6942=DIRECTION('',(1.,0.,0.));
#6943=DIRECTION('',(0.,0.,1.));
#6944=DIRECTION('',(1.,0.,0.));
#6945=DIRECTION('',(0.,0.,1.));
#6946=DIRECTION('',(1.,0.,0.));
#6947=DIRECTION('',(0.,0.,1.));
#6948=DIRECTION('',(1.,0.,0.));
#6949=DIRECTION('',(0.,0.,1.));
#6950=DIRECTION('',(1.,0.,0.));
#6951=DIRECTION('',(0.,0.,1.));
#6952=DIRECTION('',(1.,0.,0.));
#6953=DIRECTION('',(0.,0.,1.));
#6954=DIRECTION('',(1.,0.,0.));
#6955=DIRECTION('',(0.,0.,1.));
#6956=DIRECTION('',(1.,0.,0.));
#6957=DIRECTION('',(0.,0.,1.));
#6958=DIRECTION('',(1.,0.,0.));
#6959=DIRECTION('',(0.,0.,1.));
#6960=DIRECTION('',(1.,0.,0.));
#6961=DIRECTION('',(0.,0.,1.));
#6962=DIRECTION('',(1.,0.,0.));
#6963=DIRECTION('',(0.,0.,1.));
#6964=DIRECTION('',(1.,0.,0.));
#6965=DIRECTION('',(0.,0.,1.));
#6966=DIRECTION('',(1.,0.,0.));
#6967=DIRECTION('',(0.,0.,1.));
#6968=DIRECTION('',(1.,0.,0.));
#6969=DIRECTION('',(0.,0.,1.));
#6970=DIRECTION('',(1.,0.,0.));
#6971=DIRECTION('',(0.,-1.,2.22044604925031E-16));
#6972=DIRECTION('',(1.,0.,0.));
#6973=DIRECTION('',(0.,-1.,2.22044604925031E-16));
#6974=DIRECTION('',(1.,0.,0.));
#6975=DIRECTION('',(0.,-1.,2.22044604925031E-16));
#6976=DIRECTION('',(1.,0.,0.));
#6977=DIRECTION('',(0.,-1.,2.22044604925031E-16));
#6978=DIRECTION('',(1.,0.,0.));
#6979=DIRECTION('',(0.,-1.,2.22044604925031E-16));
#6980=DIRECTION('',(1.,0.,0.));
#6981=DIRECTION('',(0.,-1.,2.22044604925031E-16));
#6982=DIRECTION('',(1.,0.,0.));
#6983=DIRECTION('',(0.,-1.,2.22044604925031E-16));
#6984=DIRECTION('',(1.,0.,0.));
#6985=DIRECTION('',(0.,-1.,2.22044604925031E-16));
#6986=DIRECTION('',(1.,0.,0.));
#6987=DIRECTION('',(0.,-1.,2.22044604925031E-16));
#6988=DIRECTION('',(1.,0.,0.));
#6989=DIRECTION('',(0.,-1.,2.22044604925031E-16));
#6990=DIRECTION('',(1.,0.,0.));
#6991=DIRECTION('',(0.,-1.,2.22044604925031E-16));
#6992=DIRECTION('',(1.,0.,0.));
#6993=DIRECTION('',(0.,-1.,2.22044604925031E-16));
#6994=DIRECTION('',(1.,0.,0.));
#6995=DIRECTION('',(0.,-1.,2.22044604925031E-16));
#6996=DIRECTION('',(1.,0.,0.));
#6997=DIRECTION('',(0.,1.,2.22044604925031E-16));
#6998=DIRECTION('',(1.,0.,0.));
#6999=DIRECTION('',(0.,1.,2.22044604925031E-16));
#7000=DIRECTION('',(1.,0.,0.));
#7001=DIRECTION('',(0.,1.,2.22044604925031E-16));
#7002=DIRECTION('',(1.,0.,0.));
#7003=DIRECTION('axis',(0.,0.,1.));
#7004=DIRECTION('refdir',(1.,0.,0.));
#7005=DIRECTION('axis',(0.,0.,1.));
#7006=DIRECTION('refdir',(1.,0.,0.));
#7007=DIRECTION('center_axis',(0.,0.,1.));
#7008=DIRECTION('ref_axis',(1.,0.,0.));
#7009=DIRECTION('center_axis',(0.,0.,1.));
#7010=DIRECTION('ref_axis',(1.,0.,0.));
#7011=DIRECTION('',(0.,0.,1.));
#7012=DIRECTION('center_axis',(0.,0.,-1.));
#7013=DIRECTION('ref_axis',(1.,0.,0.));
#7014=DIRECTION('center_axis',(0.,0.,1.));
#7015=DIRECTION('ref_axis',(1.,0.,0.));
#7016=DIRECTION('center_axis',(0.,0.,1.));
#7017=DIRECTION('ref_axis',(1.,0.,0.));
#7018=DIRECTION('center_axis',(0.,0.,1.));
#7019=DIRECTION('ref_axis',(1.,0.,0.));
#7020=DIRECTION('',(0.,0.,1.));
#7021=DIRECTION('center_axis',(0.,0.,1.));
#7022=DIRECTION('ref_axis',(1.,0.,0.));
#7023=DIRECTION('center_axis',(0.,0.,1.));
#7024=DIRECTION('ref_axis',(1.,0.,0.));
#7025=DIRECTION('center_axis',(6.12323399573677E-17,0.,1.));
#7026=DIRECTION('ref_axis',(1.,0.,0.));
#7027=DIRECTION('center_axis',(0.,0.,1.));
#7028=DIRECTION('ref_axis',(1.,0.,0.));
#7029=DIRECTION('',(1.,0.,0.));
#7030=DIRECTION('center_axis',(0.,0.,1.));
#7031=DIRECTION('ref_axis',(1.,0.,0.));
#7032=DIRECTION('',(-1.,0.,0.));
#7033=DIRECTION('center_axis',(0.,0.,1.));
#7034=DIRECTION('ref_axis',(1.,0.,0.));
#7035=DIRECTION('center_axis',(0.,0.,1.));
#7036=DIRECTION('ref_axis',(-1.,-1.22464679914735E-16,0.));
#7037=DIRECTION('',(0.,0.,-1.));
#7038=DIRECTION('',(0.,0.,1.));
#7039=DIRECTION('center_axis',(0.,0.,1.));
#7040=DIRECTION('ref_axis',(1.,0.,0.));
#7041=DIRECTION('center_axis',(0.,0.,1.));
#7042=DIRECTION('ref_axis',(1.,0.,0.));
#7043=DIRECTION('',(-1.,0.,0.));
#7044=DIRECTION('',(1.,0.,0.));
#7045=DIRECTION('center_axis',(0.,0.,-1.));
#7046=DIRECTION('ref_axis',(1.,0.,0.));
#7047=DIRECTION('center_axis',(0.,-1.,0.));
#7048=DIRECTION('ref_axis',(1.,0.,0.));
#7049=DIRECTION('',(0.,0.,1.));
#7050=DIRECTION('',(1.,0.,0.));
#7051=DIRECTION('',(0.,0.,1.));
#7052=DIRECTION('',(1.,0.,0.));
#7053=DIRECTION('',(0.,0.,1.));
#7054=DIRECTION('center_axis',(0.,1.,0.));
#7055=DIRECTION('ref_axis',(1.,0.,0.));
#7056=DIRECTION('center_axis',(0.,1.,0.));
#7057=DIRECTION('ref_axis',(1.,0.,0.));
#7058=DIRECTION('center_axis',(0.,1.,0.));
#7059=DIRECTION('ref_axis',(1.,0.,0.));
#7060=DIRECTION('center_axis',(0.,1.,0.));
#7061=DIRECTION('ref_axis',(1.,0.,0.));
#7062=DIRECTION('center_axis',(0.,0.,1.));
#7063=DIRECTION('ref_axis',(-1.,1.22464679914735E-16,0.));
#7064=DIRECTION('',(0.,0.,-1.));
#7065=DIRECTION('center_axis',(0.,0.,1.));
#7066=DIRECTION('ref_axis',(1.,0.,0.));
#7067=DIRECTION('center_axis',(0.,1.,0.));
#7068=DIRECTION('ref_axis',(1.,0.,0.));
#7069=DIRECTION('',(0.,1.,0.));
#7070=DIRECTION('center_axis',(0.,-1.,0.));
#7071=DIRECTION('ref_axis',(1.,0.,0.));
#7072=DIRECTION('center_axis',(0.,1.,0.));
#7073=DIRECTION('ref_axis',(1.,0.,0.));
#7074=DIRECTION('',(0.,1.,0.));
#7075=DIRECTION('center_axis',(0.,-1.,0.));
#7076=DIRECTION('ref_axis',(1.,0.,0.));
#7077=DIRECTION('center_axis',(0.,1.,0.));
#7078=DIRECTION('ref_axis',(1.,0.,0.));
#7079=DIRECTION('',(0.,1.,0.));
#7080=DIRECTION('center_axis',(0.,-1.,0.));
#7081=DIRECTION('ref_axis',(1.,0.,0.));
#7082=DIRECTION('center_axis',(0.,1.,0.));
#7083=DIRECTION('ref_axis',(1.,0.,0.));
#7084=DIRECTION('',(0.,1.,0.));
#7085=DIRECTION('center_axis',(0.,-1.,0.));
#7086=DIRECTION('ref_axis',(1.,0.,0.));
#7087=DIRECTION('center_axis',(0.,1.,0.));
#7088=DIRECTION('ref_axis',(-1.,0.,0.));
#7089=DIRECTION('',(0.,0.,-1.));
#7090=DIRECTION('',(-1.,0.,0.));
#7091=DIRECTION('',(0.,0.,1.));
#7092=DIRECTION('',(-1.,0.,0.));
#7093=DIRECTION('center_axis',(1.,0.,0.));
#7094=DIRECTION('ref_axis',(0.,1.,0.));
#7095=DIRECTION('',(0.,1.,0.));
#7096=DIRECTION('',(0.,1.,0.));
#7097=DIRECTION('center_axis',(0.,0.,1.));
#7098=DIRECTION('ref_axis',(-1.,1.22464679914735E-16,0.));
#7099=DIRECTION('center_axis',(0.,0.,1.));
#7100=DIRECTION('ref_axis',(1.,0.,0.));
#7101=DIRECTION('center_axis',(0.,0.,1.));
#7102=DIRECTION('ref_axis',(1.,0.,0.));
#7103=DIRECTION('center_axis',(0.,0.,-1.));
#7104=DIRECTION('ref_axis',(1.,0.,0.));
#7105=DIRECTION('center_axis',(0.,0.,1.));
#7106=DIRECTION('ref_axis',(1.,0.,0.));
#7107=DIRECTION('center_axis',(0.,0.,1.));
#7108=DIRECTION('ref_axis',(1.,0.,0.));
#7109=DIRECTION('center_axis',(0.,0.,1.));
#7110=DIRECTION('ref_axis',(1.,0.,0.));
#7111=DIRECTION('',(0.,0.,-1.));
#7112=DIRECTION('center_axis',(0.,0.,1.));
#7113=DIRECTION('ref_axis',(1.,0.,0.));
#7114=DIRECTION('center_axis',(0.,0.,1.));
#7115=DIRECTION('ref_axis',(1.,0.,0.));
#7116=DIRECTION('center_axis',(0.,0.,1.));
#7117=DIRECTION('ref_axis',(1.,0.,0.));
#7118=DIRECTION('',(0.,0.,-1.));
#7119=DIRECTION('center_axis',(0.,0.,1.));
#7120=DIRECTION('ref_axis',(1.,0.,0.));
#7121=DIRECTION('center_axis',(0.,0.,1.));
#7122=DIRECTION('ref_axis',(1.,0.,0.));
#7123=DIRECTION('axis',(0.,0.,1.));
#7124=DIRECTION('refdir',(1.,0.,0.));
#7125=DIRECTION('center_axis',(0.,0.,1.));
#7126=DIRECTION('ref_axis',(1.,0.,0.));
#7127=DIRECTION('center_axis',(0.,0.,-1.));
#7128=DIRECTION('ref_axis',(1.,0.,0.));
#7129=DIRECTION('',(0.,0.,-1.));
#7130=DIRECTION('center_axis',(0.,0.,-1.));
#7131=DIRECTION('ref_axis',(1.,0.,0.));
#7132=DIRECTION('center_axis',(0.,0.,1.));
#7133=DIRECTION('ref_axis',(1.,0.,0.));
#7134=DIRECTION('center_axis',(0.,0.,1.));
#7135=DIRECTION('ref_axis',(1.,0.,0.));
#7136=DIRECTION('',(0.,0.,-1.));
#7137=DIRECTION('center_axis',(0.,0.,1.));
#7138=DIRECTION('ref_axis',(1.,0.,0.));
#7139=DIRECTION('center_axis',(0.,0.,1.));
#7140=DIRECTION('ref_axis',(1.,0.,0.));
#7141=DIRECTION('center_axis',(0.,0.,1.));
#7142=DIRECTION('ref_axis',(1.,0.,0.));
#7143=DIRECTION('axis',(0.,0.,1.));
#7144=DIRECTION('refdir',(1.,0.,0.));
#7145=DIRECTION('center_axis',(0.,0.,1.));
#7146=DIRECTION('ref_axis',(1.,0.,0.));
#7147=DIRECTION('center_axis',(0.,0.,-1.));
#7148=DIRECTION('ref_axis',(1.,0.,0.));
#7149=DIRECTION('',(0.,0.,-1.));
#7150=DIRECTION('center_axis',(0.,0.,-1.));
#7151=DIRECTION('ref_axis',(1.,0.,0.));
#7152=DIRECTION('center_axis',(0.,0.,1.));
#7153=DIRECTION('ref_axis',(1.,0.,0.));
#7154=DIRECTION('center_axis',(0.,0.,1.));
#7155=DIRECTION('ref_axis',(1.,0.,0.));
#7156=DIRECTION('',(0.,0.,-1.));
#7157=DIRECTION('center_axis',(0.,0.,1.));
#7158=DIRECTION('ref_axis',(1.,0.,0.));
#7159=DIRECTION('center_axis',(0.,0.,1.));
#7160=DIRECTION('ref_axis',(1.,0.,0.));
#7161=DIRECTION('center_axis',(0.,0.,1.));
#7162=DIRECTION('ref_axis',(1.,0.,0.));
#7163=DIRECTION('axis',(0.,0.,1.));
#7164=DIRECTION('refdir',(1.,0.,0.));
#7165=DIRECTION('center_axis',(0.,0.,1.));
#7166=DIRECTION('ref_axis',(1.,0.,0.));
#7167=DIRECTION('center_axis',(0.,0.,-1.));
#7168=DIRECTION('ref_axis',(1.,0.,0.));
#7169=DIRECTION('',(0.,0.,-1.));
#7170=DIRECTION('center_axis',(0.,0.,-1.));
#7171=DIRECTION('ref_axis',(1.,0.,0.));
#7172=DIRECTION('center_axis',(0.,0.,1.));
#7173=DIRECTION('ref_axis',(1.,0.,0.));
#7174=DIRECTION('center_axis',(0.,0.,1.));
#7175=DIRECTION('ref_axis',(1.,0.,0.));
#7176=DIRECTION('',(0.,0.,-1.));
#7177=DIRECTION('center_axis',(0.,0.,1.));
#7178=DIRECTION('ref_axis',(1.,0.,0.));
#7179=DIRECTION('center_axis',(0.,0.,1.));
#7180=DIRECTION('ref_axis',(1.,0.,0.));
#7181=DIRECTION('center_axis',(0.,0.,1.));
#7182=DIRECTION('ref_axis',(1.,0.,0.));
#7183=DIRECTION('axis',(0.,0.,1.));
#7184=DIRECTION('refdir',(1.,0.,0.));
#7185=DIRECTION('center_axis',(0.,0.,1.));
#7186=DIRECTION('ref_axis',(1.,0.,0.));
#7187=DIRECTION('center_axis',(0.,0.,-1.));
#7188=DIRECTION('ref_axis',(1.,0.,0.));
#7189=DIRECTION('',(0.,0.,-1.));
#7190=DIRECTION('center_axis',(0.,0.,-1.));
#7191=DIRECTION('ref_axis',(1.,0.,0.));
#7192=DIRECTION('center_axis',(0.,0.,1.));
#7193=DIRECTION('ref_axis',(1.,0.,0.));
#7194=DIRECTION('center_axis',(0.,0.,1.));
#7195=DIRECTION('ref_axis',(1.,0.,0.));
#7196=DIRECTION('',(0.,0.,-1.));
#7197=DIRECTION('center_axis',(0.,0.,1.));
#7198=DIRECTION('ref_axis',(1.,0.,0.));
#7199=DIRECTION('center_axis',(0.,0.,1.));
#7200=DIRECTION('ref_axis',(1.,0.,0.));
#7201=DIRECTION('center_axis',(0.,0.,1.));
#7202=DIRECTION('ref_axis',(1.,0.,0.));
#7203=DIRECTION('axis',(0.,0.,1.));
#7204=DIRECTION('refdir',(1.,0.,0.));
#7205=DIRECTION('center_axis',(0.,1.,0.));
#7206=DIRECTION('ref_axis',(0.,0.,1.));
#7207=DIRECTION('center_axis',(0.,-1.,0.));
#7208=DIRECTION('ref_axis',(1.,0.,0.));
#7209=DIRECTION('center_axis',(0.,-1.,0.));
#7210=DIRECTION('ref_axis',(1.,0.,0.));
#7211=DIRECTION('center_axis',(0.,-1.,0.));
#7212=DIRECTION('ref_axis',(1.,0.,0.));
#7213=DIRECTION('',(0.707106781186547,0.707106781186548,8.65956056235493E-17));
#7214=DIRECTION('center_axis',(0.,-1.,0.));
#7215=DIRECTION('ref_axis',(1.,0.,0.));
#7216=DIRECTION('center_axis',(0.,-1.,0.));
#7217=DIRECTION('ref_axis',(1.,0.,0.));
#7218=DIRECTION('',(0.,1.,0.));
#7219=DIRECTION('center_axis',(0.,1.,0.));
#7220=DIRECTION('ref_axis',(1.,0.,0.));
#7221=DIRECTION('center_axis',(0.,-1.,0.));
#7222=DIRECTION('ref_axis',(1.,0.,0.));
#7223=DIRECTION('',(-0.707106781186547,0.707106781186548,-8.65956056235493E-17));
#7224=DIRECTION('center_axis',(0.,-1.,0.));
#7225=DIRECTION('ref_axis',(0.,0.,-1.));
#7226=DIRECTION('center_axis',(0.,-1.,0.));
#7227=DIRECTION('ref_axis',(1.,0.,0.));
#7228=DIRECTION('center_axis',(0.,1.,0.));
#7229=DIRECTION('ref_axis',(1.,0.,0.));
#7230=DIRECTION('center_axis',(0.,1.,0.));
#7231=DIRECTION('ref_axis',(1.,0.,0.));
#7232=DIRECTION('',(-0.447213595499958,0.894427190999916,-5.47678698264203E-17));
#7233=DIRECTION('center_axis',(0.,-1.,0.));
#7234=DIRECTION('ref_axis',(1.,0.,0.));
#7235=DIRECTION('center_axis',(0.,1.,0.));
#7236=DIRECTION('ref_axis',(1.,0.,0.));
#7237=DIRECTION('',(0.,1.,0.));
#7238=DIRECTION('center_axis',(0.,1.,0.));
#7239=DIRECTION('ref_axis',(1.,0.,0.));
#7240=DIRECTION('center_axis',(0.,-1.,0.));
#7241=DIRECTION('ref_axis',(1.,0.,0.));
#7242=DIRECTION('',(-0.707106781186547,0.707106781186548,-8.65956056235493E-17));
#7243=DIRECTION('center_axis',(0.,-1.,0.));
#7244=DIRECTION('ref_axis',(0.,0.,-1.));
#7245=DIRECTION('center_axis',(0.866025403784439,0.,-0.5));
#7246=DIRECTION('ref_axis',(0.5,0.,0.866025403784439));
#7247=DIRECTION('',(-0.5,0.,-0.866025403784439));
#7248=DIRECTION('',(0.,-1.,0.));
#7249=DIRECTION('',(0.5,0.,0.866025403784439));
#7250=DIRECTION('',(0.,-1.,0.));
#7251=DIRECTION('center_axis',(1.60246890531964E-16,0.,-1.));
#7252=DIRECTION('ref_axis',(1.,0.,1.60246890531964E-16));
#7253=DIRECTION('',(-1.,0.,-1.60246890531964E-16));
#7254=DIRECTION('',(0.,-1.,0.));
#7255=DIRECTION('',(1.,0.,1.60246890531964E-16));
#7256=DIRECTION('center_axis',(-0.866025403784439,0.,-0.5));
#7257=DIRECTION('ref_axis',(0.5,0.,-0.866025403784439));
#7258=DIRECTION('',(-0.5,0.,0.866025403784439));
#7259=DIRECTION('',(0.,-1.,0.));
#7260=DIRECTION('',(0.5,0.,-0.866025403784439));
#7261=DIRECTION('center_axis',(-0.866025403784439,0.,0.5));
#7262=DIRECTION('ref_axis',(-0.5,0.,-0.866025403784439));
#7263=DIRECTION('',(0.5,0.,0.866025403784439));
#7264=DIRECTION('',(0.,-1.,0.));
#7265=DIRECTION('',(-0.5,0.,-0.866025403784439));
#7266=DIRECTION('center_axis',(-1.60246890531964E-16,0.,1.));
#7267=DIRECTION('ref_axis',(-1.,0.,-1.60246890531964E-16));
#7268=DIRECTION('',(1.,0.,1.60246890531964E-16));
#7269=DIRECTION('',(0.,-1.,0.));
#7270=DIRECTION('',(-1.,0.,-1.60246890531964E-16));
#7271=DIRECTION('center_axis',(0.866025403784439,0.,0.5));
#7272=DIRECTION('ref_axis',(-0.5,0.,0.866025403784439));
#7273=DIRECTION('',(0.5,0.,-0.866025403784439));
#7274=DIRECTION('',(-0.5,0.,0.866025403784439));
#7275=DIRECTION('center_axis',(0.,1.,0.));
#7276=DIRECTION('ref_axis',(1.,0.,0.));
#7277=DIRECTION('center_axis',(0.,-1.,0.));
#7278=DIRECTION('ref_axis',(0.,0.,-1.));
#7279=DIRECTION('',(0.,0.,1.));
#7280=DIRECTION('',(1.,0.,0.));
#7281=DIRECTION('',(0.,0.,1.));
#7282=DIRECTION('',(1.,0.,0.));
#7283=DIRECTION('',(0.,0.,1.));
#7284=DIRECTION('',(1.,0.,0.));
#7285=DIRECTION('',(0.,0.,1.));
#7286=DIRECTION('',(1.,0.,0.));
#7287=DIRECTION('',(0.,0.,1.));
#7288=DIRECTION('',(1.,0.,0.));
#7289=DIRECTION('',(0.,1.,2.22044604925031E-16));
#7290=DIRECTION('',(1.,0.,0.));
#7291=DIRECTION('',(0.,-1.,2.22044604925031E-16));
#7292=DIRECTION('',(1.,0.,0.));
#7293=DIRECTION('',(0.,0.,1.));
#7294=DIRECTION('',(1.,0.,0.));
#7295=DIRECTION('',(0.,0.,1.));
#7296=DIRECTION('',(1.,0.,0.));
#7297=CARTESIAN_POINT('',(0.,0.,0.));
#7298=CARTESIAN_POINT('',(0.,0.,0.));
#7299=CARTESIAN_POINT('',(0.,0.,0.));
#7300=CARTESIAN_POINT('Origin',(-2.2,-1.8,-1.1));
#7301=CARTESIAN_POINT('',(-2.45,-1.8,-1.));
#7302=CARTESIAN_POINT('Origin',(-2.2,-1.8,-1.));
#7303=CARTESIAN_POINT('',(-2.45,-1.8,0.));
#7304=CARTESIAN_POINT('',(-2.45,-1.8,-1.1));
#7305=CARTESIAN_POINT('Origin',(-2.2,-1.8,0.));
#7306=CARTESIAN_POINT('Origin',(-5.3,1.8,-1.1));
#7307=CARTESIAN_POINT('',(-5.55,1.8,-1.));
#7308=CARTESIAN_POINT('Origin',(-5.3,1.8,-1.));
#7309=CARTESIAN_POINT('',(-5.55,1.8,0.));
#7310=CARTESIAN_POINT('',(-5.55,1.8,-1.1));
#7311=CARTESIAN_POINT('Origin',(-5.3,1.8,0.));
#7312=CARTESIAN_POINT('Origin',(-5.3,-1.8,-1.1));
#7313=CARTESIAN_POINT('',(-5.55,-1.8,-1.));
#7314=CARTESIAN_POINT('Origin',(-5.3,-1.8,-1.));
#7315=CARTESIAN_POINT('',(-5.55,-1.8,0.));
#7316=CARTESIAN_POINT('',(-5.55,-1.8,-1.1));
#7317=CARTESIAN_POINT('Origin',(-5.3,-1.8,0.));
#7318=CARTESIAN_POINT('Origin',(-2.2,1.8,-1.1));
#7319=CARTESIAN_POINT('',(-2.45,1.8,-1.));
#7320=CARTESIAN_POINT('Origin',(-2.2,1.8,-1.));
#7321=CARTESIAN_POINT('',(-2.45,1.8,0.));
#7322=CARTESIAN_POINT('',(-2.45,1.8,-1.1));
#7323=CARTESIAN_POINT('Origin',(-2.2,1.8,0.));
#7324=CARTESIAN_POINT('Origin',(13.5,13.5,-1.));
#7325=CARTESIAN_POINT('',(13.5,13.5,-1.));
#7326=CARTESIAN_POINT('',(-14.5,13.5,-1.));
#7327=CARTESIAN_POINT('',(13.5,13.5,-1.));
#7328=CARTESIAN_POINT('',(-14.5,13.5,0.));
#7329=CARTESIAN_POINT('',(-14.5,13.5,-1.));
#7330=CARTESIAN_POINT('',(13.5,13.5,0.));
#7331=CARTESIAN_POINT('',(13.5,13.5,0.));
#7332=CARTESIAN_POINT('',(13.5,13.5,-1.));
#7333=CARTESIAN_POINT('Origin',(13.5,-6.5,-1.));
#7334=CARTESIAN_POINT('',(13.5,-6.5,-1.));
#7335=CARTESIAN_POINT('',(13.5,-6.5,-1.));
#7336=CARTESIAN_POINT('',(13.5,-6.5,0.));
#7337=CARTESIAN_POINT('',(13.5,-6.5,0.));
#7338=CARTESIAN_POINT('',(13.5,-6.5,-1.));
#7339=CARTESIAN_POINT('Origin',(-14.5,-6.5,-1.));
#7340=CARTESIAN_POINT('',(-14.5,-6.5,-1.));
#7341=CARTESIAN_POINT('',(-14.5,-6.5,-1.));
#7342=CARTESIAN_POINT('',(-14.5,-6.5,0.));
#7343=CARTESIAN_POINT('',(-14.5,-6.5,0.));
#7344=CARTESIAN_POINT('',(-14.5,-6.5,-1.));
#7345=CARTESIAN_POINT('Origin',(-14.5,13.5,-1.));
#7346=CARTESIAN_POINT('',(-14.5,13.5,-1.));
#7347=CARTESIAN_POINT('',(-14.5,13.5,0.));
#7348=CARTESIAN_POINT('Origin',(-0.5,3.5,0.));
#7349=CARTESIAN_POINT('Origin',(-0.5,3.5,-1.));
#7350=CARTESIAN_POINT('',(0.,0.,0.));
#7351=CARTESIAN_POINT('Origin',(-11.5,13.5,-1.4));
#7352=CARTESIAN_POINT('',(-11.5,13.5,-1.4));
#7353=CARTESIAN_POINT('',(-13.5,13.5,-1.4));
#7354=CARTESIAN_POINT('',(-11.5,13.5,-1.4));
#7355=CARTESIAN_POINT('',(-13.5,13.5,-1.));
#7356=CARTESIAN_POINT('',(-13.5,13.5,-1.4));
#7357=CARTESIAN_POINT('',(-11.5,13.5,-1.));
#7358=CARTESIAN_POINT('',(-11.5,13.5,-1.));
#7359=CARTESIAN_POINT('',(-11.5,13.5,-1.4));
#7360=CARTESIAN_POINT('Origin',(-11.5,-6.5,-1.4));
#7361=CARTESIAN_POINT('',(-11.5,-6.5,-1.4));
#7362=CARTESIAN_POINT('',(-11.5,-6.5,-1.4));
#7363=CARTESIAN_POINT('',(-11.5,-6.5,-1.));
#7364=CARTESIAN_POINT('',(-11.5,-6.5,-1.));
#7365=CARTESIAN_POINT('',(-11.5,-6.5,-1.4));
#7366=CARTESIAN_POINT('Origin',(-13.5,-6.5,-1.4));
#7367=CARTESIAN_POINT('',(-13.5,-6.5,-1.4));
#7368=CARTESIAN_POINT('',(-13.5,-6.5,-1.4));
#7369=CARTESIAN_POINT('',(-13.5,-6.5,-1.));
#7370=CARTESIAN_POINT('',(-13.5,-6.5,-1.));
#7371=CARTESIAN_POINT('',(-13.5,-6.5,-1.4));
#7372=CARTESIAN_POINT('Origin',(-13.5,13.5,-1.4));
#7373=CARTESIAN_POINT('',(-13.5,13.5,-1.4));
#7374=CARTESIAN_POINT('',(-13.5,13.5,-1.));
#7375=CARTESIAN_POINT('Origin',(-12.5,3.5,-1.));
#7376=CARTESIAN_POINT('Origin',(-12.5,3.5,-1.4));
#7377=CARTESIAN_POINT('',(0.,0.,0.));
#7378=CARTESIAN_POINT('Origin',(13.5,13.5,-1.4));
#7379=CARTESIAN_POINT('',(13.5,13.5,-1.4));
#7380=CARTESIAN_POINT('',(11.5,13.5,-1.4));
#7381=CARTESIAN_POINT('',(13.5,13.5,-1.4));
#7382=CARTESIAN_POINT('',(11.5,13.5,-1.));
#7383=CARTESIAN_POINT('',(11.5,13.5,-1.4));
#7384=CARTESIAN_POINT('',(13.5,13.5,-1.));
#7385=CARTESIAN_POINT('',(13.5,13.5,-1.));
#7386=CARTESIAN_POINT('',(13.5,13.5,-1.4));
#7387=CARTESIAN_POINT('Origin',(13.5,-6.5,-1.4));
#7388=CARTESIAN_POINT('',(13.5,-6.5,-1.4));
#7389=CARTESIAN_POINT('',(13.5,-6.5,-1.4));
#7390=CARTESIAN_POINT('',(13.5,-6.5,-1.));
#7391=CARTESIAN_POINT('',(13.5,-6.5,-1.));
#7392=CARTESIAN_POINT('',(13.5,-6.5,-1.4));
#7393=CARTESIAN_POINT('Origin',(11.5,-6.5,-1.4));
#7394=CARTESIAN_POINT('',(11.5,-6.5,-1.4));
#7395=CARTESIAN_POINT('',(11.5,-6.5,-1.4));
#7396=CARTESIAN_POINT('',(11.5,-6.5,-1.));
#7397=CARTESIAN_POINT('',(11.5,-6.5,-1.));
#7398=CARTESIAN_POINT('',(11.5,-6.5,-1.4));
#7399=CARTESIAN_POINT('Origin',(11.5,13.5,-1.4));
#7400=CARTESIAN_POINT('',(11.5,13.5,-1.4));
#7401=CARTESIAN_POINT('',(11.5,13.5,-1.));
#7402=CARTESIAN_POINT('Origin',(12.5,3.5,-1.));
#7403=CARTESIAN_POINT('Origin',(12.5,3.5,-1.4));
#7404=CARTESIAN_POINT('',(0.,0.,0.));
#7405=CARTESIAN_POINT('Origin',(-3.,1.5,0.8));
#7406=CARTESIAN_POINT('',(-3.,1.5,0.8));
#7407=CARTESIAN_POINT('',(-4.5,1.5,0.8));
#7408=CARTESIAN_POINT('',(-3.,1.5,0.8));
#7409=CARTESIAN_POINT('',(-4.5,1.5,13.));
#7410=CARTESIAN_POINT('',(-4.5,1.5,0.8));
#7411=CARTESIAN_POINT('',(-3.,1.5,13.));
#7412=CARTESIAN_POINT('',(-3.,1.5,13.));
#7413=CARTESIAN_POINT('',(-3.,1.5,0.8));
#7414=CARTESIAN_POINT('Origin',(-3.,-1.5,0.8));
#7415=CARTESIAN_POINT('',(-3.,-1.5,0.8));
#7416=CARTESIAN_POINT('',(-3.,-1.5,0.8));
#7417=CARTESIAN_POINT('',(-3.,-1.5,13.));
#7418=CARTESIAN_POINT('',(-3.,-1.5,13.));
#7419=CARTESIAN_POINT('',(-3.,-1.5,0.8));
#7420=CARTESIAN_POINT('Origin',(-4.5,-1.5,0.8));
#7421=CARTESIAN_POINT('',(-4.5,-1.5,0.8));
#7422=CARTESIAN_POINT('',(-4.5,-1.5,0.8));
#7423=CARTESIAN_POINT('',(-4.5,-1.5,13.));
#7424=CARTESIAN_POINT('',(-4.5,-1.5,13.));
#7425=CARTESIAN_POINT('',(-4.5,-1.5,0.8));
#7426=CARTESIAN_POINT('Origin',(-4.5,1.5,0.8));
#7427=CARTESIAN_POINT('',(-4.5,1.5,0.8));
#7428=CARTESIAN_POINT('',(-4.5,1.5,13.));
#7429=CARTESIAN_POINT('Origin',(-3.75,0.,13.));
#7430=CARTESIAN_POINT('Origin',(-3.75,0.,0.8));
#7431=CARTESIAN_POINT('Origin',(-2.2,-1.8,-0.1));
#7432=CARTESIAN_POINT('',(-2.53,-1.8,0.));
#7433=CARTESIAN_POINT('Origin',(-2.2,-1.8,0.));
#7434=CARTESIAN_POINT('',(-2.53,-1.8,0.8));
#7435=CARTESIAN_POINT('',(-2.53,-1.8,-0.1));
#7436=CARTESIAN_POINT('Origin',(-2.2,-1.8,0.8));
#7437=CARTESIAN_POINT('Origin',(-5.3,1.8,-0.1));
#7438=CARTESIAN_POINT('',(-5.63,1.8,0.));
#7439=CARTESIAN_POINT('Origin',(-5.3,1.8,0.));
#7440=CARTESIAN_POINT('',(-5.63,1.8,0.8));
#7441=CARTESIAN_POINT('',(-5.63,1.8,-0.1));
#7442=CARTESIAN_POINT('Origin',(-5.3,1.8,0.8));
#7443=CARTESIAN_POINT('Origin',(-5.3,-1.8,-0.1));
#7444=CARTESIAN_POINT('',(-5.63,-1.8,0.));
#7445=CARTESIAN_POINT('Origin',(-5.3,-1.8,0.));
#7446=CARTESIAN_POINT('',(-5.63,-1.8,0.8));
#7447=CARTESIAN_POINT('',(-5.63,-1.8,-0.1));
#7448=CARTESIAN_POINT('Origin',(-5.3,-1.8,0.8));
#7449=CARTESIAN_POINT('Origin',(-2.2,1.8,-0.1));
#7450=CARTESIAN_POINT('',(-2.53,1.8,0.));
#7451=CARTESIAN_POINT('Origin',(-2.2,1.8,0.));
#7452=CARTESIAN_POINT('',(-2.53,1.8,0.8));
#7453=CARTESIAN_POINT('',(-2.53,1.8,-0.1));
#7454=CARTESIAN_POINT('Origin',(-2.2,1.8,0.8));
#7455=CARTESIAN_POINT('Origin',(-1.5,2.5,0.));
#7456=CARTESIAN_POINT('',(-1.5,2.5,0.));
#7457=CARTESIAN_POINT('',(-6.,2.5,0.));
#7458=CARTESIAN_POINT('',(-1.5,2.5,0.));
#7459=CARTESIAN_POINT('',(-6.,2.5,0.8));
#7460=CARTESIAN_POINT('',(-6.,2.5,0.));
#7461=CARTESIAN_POINT('',(-1.5,2.5,0.8));
#7462=CARTESIAN_POINT('',(-1.5,2.5,0.8));
#7463=CARTESIAN_POINT('',(-1.5,2.5,0.));
#7464=CARTESIAN_POINT('Origin',(-1.5,-2.5,0.));
#7465=CARTESIAN_POINT('',(-1.5,-2.5,0.));
#7466=CARTESIAN_POINT('',(-1.5,-2.5,0.));
#7467=CARTESIAN_POINT('',(-1.5,-2.5,0.8));
#7468=CARTESIAN_POINT('',(-1.5,-2.5,0.8));
#7469=CARTESIAN_POINT('',(-1.5,-2.5,0.));
#7470=CARTESIAN_POINT('Origin',(-6.,-2.5,0.));
#7471=CARTESIAN_POINT('',(-6.,-2.5,0.));
#7472=CARTESIAN_POINT('',(-6.,-2.5,0.));
#7473=CARTESIAN_POINT('',(-6.,-2.5,0.8));
#7474=CARTESIAN_POINT('',(-6.,-2.5,0.8));
#7475=CARTESIAN_POINT('',(-6.,-2.5,0.));
#7476=CARTESIAN_POINT('Origin',(-6.,2.5,0.));
#7477=CARTESIAN_POINT('',(-6.,2.5,0.));
#7478=CARTESIAN_POINT('',(-6.,2.5,0.8));
#7479=CARTESIAN_POINT('Origin',(-3.75,0.,0.8));
#7480=CARTESIAN_POINT('Origin',(-3.75,0.,0.));
#7481=CARTESIAN_POINT('',(0.,0.,0.));
#7482=CARTESIAN_POINT('Origin',(-6.5,-0.4,5.5));
#7483=CARTESIAN_POINT('',(-6.83,-0.3,5.5));
#7484=CARTESIAN_POINT('Origin',(-6.5,-0.3,5.5));
#7485=CARTESIAN_POINT('',(-6.83,0.3,5.5));
#7486=CARTESIAN_POINT('',(-6.83,-0.4,5.5));
#7487=CARTESIAN_POINT('Origin',(-6.5,0.3,5.5));
#7488=CARTESIAN_POINT('Origin',(-12.5,-0.4,8.5));
#7489=CARTESIAN_POINT('',(-12.83,-0.3,8.5));
#7490=CARTESIAN_POINT('Origin',(-12.5,-0.3,8.5));
#7491=CARTESIAN_POINT('',(-12.83,0.3,8.5));
#7492=CARTESIAN_POINT('',(-12.83,-0.4,8.5));
#7493=CARTESIAN_POINT('Origin',(-12.5,0.3,8.5));
#7494=CARTESIAN_POINT('Origin',(-12.5,-0.4,5.5));
#7495=CARTESIAN_POINT('',(-12.83,-0.3,5.5));
#7496=CARTESIAN_POINT('Origin',(-12.5,-0.3,5.5));
#7497=CARTESIAN_POINT('',(-12.83,0.3,5.5));
#7498=CARTESIAN_POINT('',(-12.83,-0.4,5.5));
#7499=CARTESIAN_POINT('Origin',(-12.5,0.3,5.5));
#7500=CARTESIAN_POINT('Origin',(-6.5,-0.4,8.5));
#7501=CARTESIAN_POINT('',(-6.83,-0.3,8.5));
#7502=CARTESIAN_POINT('Origin',(-6.5,-0.3,8.5));
#7503=CARTESIAN_POINT('',(-6.83,0.3,8.5));
#7504=CARTESIAN_POINT('',(-6.83,-0.4,8.5));
#7505=CARTESIAN_POINT('Origin',(-6.5,0.3,8.5));
#7506=CARTESIAN_POINT('Origin',(-4.5,0.3,4.));
#7507=CARTESIAN_POINT('',(-4.5,0.3,4.));
#7508=CARTESIAN_POINT('',(-14.5,0.3,4.));
#7509=CARTESIAN_POINT('',(-4.5,0.3,4.));
#7510=CARTESIAN_POINT('',(-14.5,0.3,10.));
#7511=CARTESIAN_POINT('',(-14.5,0.3,4.));
#7512=CARTESIAN_POINT('',(-4.5,0.3,10.));
#7513=CARTESIAN_POINT('',(-4.5,0.3,10.));
#7514=CARTESIAN_POINT('',(-4.5,0.3,4.));
#7515=CARTESIAN_POINT('Origin',(-4.5,-0.3,4.));
#7516=CARTESIAN_POINT('',(-4.5,-0.3,4.));
#7517=CARTESIAN_POINT('',(-4.5,-0.3,4.));
#7518=CARTESIAN_POINT('',(-4.5,-0.3,10.));
#7519=CARTESIAN_POINT('',(-4.5,-0.3,10.));
#7520=CARTESIAN_POINT('',(-4.5,-0.3,4.));
#7521=CARTESIAN_POINT('Origin',(-14.5,-0.3,4.));
#7522=CARTESIAN_POINT('',(-14.5,-0.3,4.));
#7523=CARTESIAN_POINT('',(-14.5,-0.3,4.));
#7524=CARTESIAN_POINT('',(-14.5,-0.3,10.));
#7525=CARTESIAN_POINT('',(-14.5,-0.3,10.));
#7526=CARTESIAN_POINT('',(-14.5,-0.3,4.));
#7527=CARTESIAN_POINT('Origin',(-14.5,0.3,4.));
#7528=CARTESIAN_POINT('',(-14.5,0.3,4.));
#7529=CARTESIAN_POINT('',(-14.5,0.3,10.));
#7530=CARTESIAN_POINT('Origin',(-9.5,0.,10.));
#7531=CARTESIAN_POINT('Origin',(-9.5,0.,4.));
#7532=CARTESIAN_POINT('',(0.,0.,0.));
#7533=CARTESIAN_POINT('Origin',(1.75,0.,1.9));
#7534=CARTESIAN_POINT('',(1.585,-2.02066721859313E-17,2.));
#7535=CARTESIAN_POINT('Origin',(1.75,0.,2.));
#7536=CARTESIAN_POINT('',(1.585,2.02066721859313E-17,3.4));
#7537=CARTESIAN_POINT('',(1.585,-2.02066721859313E-17,1.9));
#7538=CARTESIAN_POINT('Origin',(1.75,0.,3.4));
#7539=CARTESIAN_POINT('Origin',(-0.875,1.51554445662277,1.9));
#7540=CARTESIAN_POINT('',(-1.04,1.51554445662277,2.));
#7541=CARTESIAN_POINT('Origin',(-0.875,1.51554445662277,2.));
#7542=CARTESIAN_POINT('',(-1.04,1.51554445662277,3.4));
#7543=CARTESIAN_POINT('',(-1.04,1.51554445662277,1.9));
#7544=CARTESIAN_POINT('Origin',(-0.875,1.51554445662277,3.4));
#7545=CARTESIAN_POINT('Origin',(-0.875000000000001,-1.51554445662277,1.9));
#7546=CARTESIAN_POINT('',(-1.04,-1.51554445662277,2.));
#7547=CARTESIAN_POINT('Origin',(-0.875000000000001,-1.51554445662277,2.));
#7548=CARTESIAN_POINT('',(-1.04,-1.51554445662277,3.4));
#7549=CARTESIAN_POINT('',(-1.04,-1.51554445662277,1.9));
#7550=CARTESIAN_POINT('Origin',(-0.875000000000001,-1.51554445662277,3.4));
#7551=CARTESIAN_POINT('Origin',(0.,0.,2.5));
#7552=CARTESIAN_POINT('',(-1.5,-1.83697019872103E-16,2.5));
#7553=CARTESIAN_POINT('Origin',(0.,0.,2.5));
#7554=CARTESIAN_POINT('',(-1.5,1.83697019872103E-16,3.4));
#7555=CARTESIAN_POINT('',(-1.5,-1.83697019872103E-16,2.5));
#7556=CARTESIAN_POINT('Origin',(0.,0.,3.4));
#7557=CARTESIAN_POINT('Origin',(0.,0.,2.5));
#7558=CARTESIAN_POINT('',(-1.02,-1.2491397351303E-16,2.5));
#7559=CARTESIAN_POINT('Origin',(0.,0.,2.5));
#7560=CARTESIAN_POINT('Origin',(0.,0.,1.9));
#7561=CARTESIAN_POINT('',(-1.02,-1.2491397351303E-16,2.));
#7562=CARTESIAN_POINT('Origin',(0.,0.,2.));
#7563=CARTESIAN_POINT('',(-1.02,-1.2491397351303E-16,1.9));
#7564=CARTESIAN_POINT('Origin',(0.,0.,3.4));
#7565=CARTESIAN_POINT('',(-1.84661853126194,1.,3.4));
#7566=CARTESIAN_POINT('',(-3.,1.,3.4));
#7567=CARTESIAN_POINT('',(0.,1.,3.4));
#7568=CARTESIAN_POINT('',(-3.,-1.,3.4));
#7569=CARTESIAN_POINT('',(-3.,1.,3.4));
#7570=CARTESIAN_POINT('',(-1.84661853126194,-1.,3.4));
#7571=CARTESIAN_POINT('',(-3.,-1.,3.4));
#7572=CARTESIAN_POINT('Origin',(0.,0.,3.4));
#7573=CARTESIAN_POINT('Origin',(0.,1.,2.));
#7574=CARTESIAN_POINT('',(-1.84661853126194,1.,2.));
#7575=CARTESIAN_POINT('',(-1.84661853126194,1.,2.));
#7576=CARTESIAN_POINT('',(-3.,1.,2.));
#7577=CARTESIAN_POINT('',(0.,1.,2.));
#7578=CARTESIAN_POINT('',(-3.,1.,2.));
#7579=CARTESIAN_POINT('Origin',(-3.,-1.,2.));
#7580=CARTESIAN_POINT('',(-1.84661853126194,-1.,2.));
#7581=CARTESIAN_POINT('',(-1.84661853126194,-1.,2.));
#7582=CARTESIAN_POINT('',(-3.,-1.,2.));
#7583=CARTESIAN_POINT('',(-3.,-1.,2.));
#7584=CARTESIAN_POINT('',(-3.,-1.,2.));
#7585=CARTESIAN_POINT('Origin',(-3.,1.,2.));
#7586=CARTESIAN_POINT('',(-3.,1.,2.));
#7587=CARTESIAN_POINT('Origin',(0.,0.,2.));
#7588=CARTESIAN_POINT('Origin',(0.,0.,2.));
#7589=CARTESIAN_POINT('Origin',(0.,0.,2.));
#7590=CARTESIAN_POINT('',(0.,0.,0.));
#7591=CARTESIAN_POINT('Origin',(1.75,0.,3.6));
#7592=CARTESIAN_POINT('',(2.09482142857143,0.14738786380825,3.6));
#7593=CARTESIAN_POINT('',(2.09482142857143,-0.14738786380825,3.6));
#7594=CARTESIAN_POINT('Origin',(0.,0.,3.6));
#7595=CARTESIAN_POINT('Origin',(1.75,0.,3.6));
#7596=CARTESIAN_POINT('',(1.525,-2.75545529808155E-17,3.6));
#7597=CARTESIAN_POINT('Origin',(1.75,0.,3.6));
#7598=CARTESIAN_POINT('Origin',(1.75,0.,3.6));
#7599=CARTESIAN_POINT('',(2.09482142857143,0.147387863808251,4.));
#7600=CARTESIAN_POINT('',(2.09482142857143,0.14738786380825,3.6));
#7601=CARTESIAN_POINT('',(2.09482142857143,-0.147387863808251,4.));
#7602=CARTESIAN_POINT('Origin',(1.75,0.,4.));
#7603=CARTESIAN_POINT('',(2.09482142857143,-0.14738786380825,3.6));
#7604=CARTESIAN_POINT('Origin',(-0.875,1.51554445662277,3.6));
#7605=CARTESIAN_POINT('',(-1.17505234855318,1.74047464163074,3.6));
#7606=CARTESIAN_POINT('',(-0.919769080018249,1.88786250543899,3.6));
#7607=CARTESIAN_POINT('Origin',(0.,0.,3.6));
#7608=CARTESIAN_POINT('Origin',(-0.875,1.51554445662277,3.6));
#7609=CARTESIAN_POINT('',(-1.1,1.51554445662277,3.6));
#7610=CARTESIAN_POINT('Origin',(-0.875,1.51554445662277,3.6));
#7611=CARTESIAN_POINT('Origin',(-0.875,1.51554445662277,3.6));
#7612=CARTESIAN_POINT('',(-1.17505234855318,1.74047464163074,4.));
#7613=CARTESIAN_POINT('',(-1.17505234855318,1.74047464163074,3.6));
#7614=CARTESIAN_POINT('',(-0.919769080018247,1.88786250543899,4.));
#7615=CARTESIAN_POINT('Origin',(-0.875,1.51554445662277,4.));
#7616=CARTESIAN_POINT('',(-0.919769080018249,1.88786250543899,3.6));
#7617=CARTESIAN_POINT('Origin',(-0.875000000000001,-1.51554445662277,3.6));
#7618=CARTESIAN_POINT('',(-0.91976908001825,-1.88786250543899,3.6));
#7619=CARTESIAN_POINT('',(-1.17505234855318,-1.74047464163074,3.6));
#7620=CARTESIAN_POINT('Origin',(0.,0.,3.6));
#7621=CARTESIAN_POINT('Origin',(-0.875000000000001,-1.51554445662277,3.6));
#7622=CARTESIAN_POINT('',(-1.1,-1.51554445662277,3.6));
#7623=CARTESIAN_POINT('Origin',(-0.875000000000001,-1.51554445662277,3.6));
#7624=CARTESIAN_POINT('Origin',(-0.875000000000001,-1.51554445662277,3.6));
#7625=CARTESIAN_POINT('',(-0.919769080018249,-1.88786250543899,4.));
#7626=CARTESIAN_POINT('',(-0.91976908001825,-1.88786250543899,3.6));
#7627=CARTESIAN_POINT('',(-1.17505234855318,-1.74047464163074,4.));
#7628=CARTESIAN_POINT('Origin',(-0.875000000000001,-1.51554445662277,4.));
#7629=CARTESIAN_POINT('',(-1.17505234855318,-1.74047464163074,3.6));
#7630=CARTESIAN_POINT('Origin',(0.,0.,3.4));
#7631=CARTESIAN_POINT('Origin',(0.,0.,4.));
#7632=CARTESIAN_POINT('',(-2.1,-2.57175827820944E-16,4.));
#7633=CARTESIAN_POINT('Origin',(0.,0.,4.));
#7634=CARTESIAN_POINT('',(-2.1,-2.57175827820944E-16,3.4));
#7635=CARTESIAN_POINT('',(-2.1,-2.57175827820944E-16,3.4));
#7636=CARTESIAN_POINT('Origin',(0.,0.,3.4));
#7637=CARTESIAN_POINT('Origin',(0.,0.,4.));
#7638=CARTESIAN_POINT('Origin',(0.,0.,4.));
#7639=CARTESIAN_POINT('Origin',(1.75,0.,3.3));
#7640=CARTESIAN_POINT('',(1.525,-2.75545529808155E-17,3.4));
#7641=CARTESIAN_POINT('Origin',(1.75,0.,3.4));
#7642=CARTESIAN_POINT('',(1.525,-2.75545529808155E-17,3.3));
#7643=CARTESIAN_POINT('Origin',(-0.875,1.51554445662277,3.3));
#7644=CARTESIAN_POINT('',(-1.1,1.51554445662277,3.4));
#7645=CARTESIAN_POINT('Origin',(-0.875,1.51554445662277,3.4));
#7646=CARTESIAN_POINT('',(-1.1,1.51554445662277,3.3));
#7647=CARTESIAN_POINT('Origin',(-0.875000000000001,-1.51554445662277,3.3));
#7648=CARTESIAN_POINT('',(-1.1,-1.51554445662277,3.4));
#7649=CARTESIAN_POINT('Origin',(-0.875000000000001,-1.51554445662277,3.4));
#7650=CARTESIAN_POINT('',(-1.1,-1.51554445662277,3.3));
#7651=CARTESIAN_POINT('Origin',(0.,0.,3.4));
#7652=CARTESIAN_POINT('',(-1.02,-1.2491397351303E-16,4.));
#7653=CARTESIAN_POINT('Origin',(0.,0.,4.));
#7654=CARTESIAN_POINT('',(-1.02,-1.2491397351303E-16,3.4));
#7655=CARTESIAN_POINT('',(-1.02,-1.2491397351303E-16,3.4));
#7656=CARTESIAN_POINT('Origin',(0.,0.,3.4));
#7657=CARTESIAN_POINT('Origin',(0.,0.,4.));
#7658=CARTESIAN_POINT('Origin',(0.,0.,3.4));
#7659=CARTESIAN_POINT('',(0.,0.,0.));
#7660=CARTESIAN_POINT('Origin',(1.75,0.,10.5));
#7661=CARTESIAN_POINT('',(1.585,-2.02066721859313E-17,10.6));
#7662=CARTESIAN_POINT('Origin',(1.75,0.,10.6));
#7663=CARTESIAN_POINT('',(1.585,2.02066721859313E-17,12.));
#7664=CARTESIAN_POINT('',(1.585,-2.02066721859313E-17,10.5));
#7665=CARTESIAN_POINT('Origin',(1.75,0.,12.));
#7666=CARTESIAN_POINT('Origin',(-0.875,1.51554445662277,10.5));
#7667=CARTESIAN_POINT('',(-1.04,1.51554445662277,10.6));
#7668=CARTESIAN_POINT('Origin',(-0.875,1.51554445662277,10.6));
#7669=CARTESIAN_POINT('',(-1.04,1.51554445662277,12.));
#7670=CARTESIAN_POINT('',(-1.04,1.51554445662277,10.5));
#7671=CARTESIAN_POINT('Origin',(-0.875,1.51554445662277,12.));
#7672=CARTESIAN_POINT('Origin',(-0.875000000000001,-1.51554445662277,10.5));
#7673=CARTESIAN_POINT('',(-1.04,-1.51554445662277,10.6));
#7674=CARTESIAN_POINT('Origin',(-0.875000000000001,-1.51554445662277,10.6));
#7675=CARTESIAN_POINT('',(-1.04,-1.51554445662277,12.));
#7676=CARTESIAN_POINT('',(-1.04,-1.51554445662277,10.5));
#7677=CARTESIAN_POINT('Origin',(-0.875000000000001,-1.51554445662277,12.));
#7678=CARTESIAN_POINT('Origin',(0.,0.,10.5));
#7679=CARTESIAN_POINT('',(-1.5,-1.83697019872103E-16,10.6));
#7680=CARTESIAN_POINT('Origin',(0.,0.,10.6));
#7681=CARTESIAN_POINT('',(-1.5,-1.83697019872103E-16,11.5));
#7682=CARTESIAN_POINT('',(-1.5,-1.83697019872103E-16,10.5));
#7683=CARTESIAN_POINT('Origin',(0.,0.,11.5));
#7684=CARTESIAN_POINT('Origin',(0.,0.,11.5));
#7685=CARTESIAN_POINT('',(-1.02,1.2491397351303E-16,11.5));
#7686=CARTESIAN_POINT('Origin',(0.,0.,11.5));
#7687=CARTESIAN_POINT('Origin',(0.,0.,10.5));
#7688=CARTESIAN_POINT('',(-1.02,1.2491397351303E-16,12.));
#7689=CARTESIAN_POINT('',(-1.02,-1.2491397351303E-16,10.5));
#7690=CARTESIAN_POINT('Origin',(0.,0.,12.));
#7691=CARTESIAN_POINT('Origin',(0.,0.,12.));
#7692=CARTESIAN_POINT('',(-1.84661853126194,1.,12.));
#7693=CARTESIAN_POINT('',(-3.,1.,12.));
#7694=CARTESIAN_POINT('',(0.,1.,12.));
#7695=CARTESIAN_POINT('',(-3.,-1.,12.));
#7696=CARTESIAN_POINT('',(-3.,1.,12.));
#7697=CARTESIAN_POINT('',(-1.84661853126194,-1.,12.));
#7698=CARTESIAN_POINT('',(-3.,-1.,12.));
#7699=CARTESIAN_POINT('Origin',(0.,0.,12.));
#7700=CARTESIAN_POINT('Origin',(0.,1.,10.6));
#7701=CARTESIAN_POINT('',(-1.84661853126194,1.,10.6));
#7702=CARTESIAN_POINT('',(-1.84661853126194,1.,10.6));
#7703=CARTESIAN_POINT('',(-3.,1.,10.6));
#7704=CARTESIAN_POINT('',(0.,1.,10.6));
#7705=CARTESIAN_POINT('',(-3.,1.,10.6));
#7706=CARTESIAN_POINT('Origin',(-3.,-1.,10.6));
#7707=CARTESIAN_POINT('',(-1.84661853126194,-1.,10.6));
#7708=CARTESIAN_POINT('',(-1.84661853126194,-1.,10.6));
#7709=CARTESIAN_POINT('',(-3.,-1.,10.6));
#7710=CARTESIAN_POINT('',(-3.,-1.,10.6));
#7711=CARTESIAN_POINT('',(-3.,-1.,10.6));
#7712=CARTESIAN_POINT('Origin',(-3.,1.,10.6));
#7713=CARTESIAN_POINT('',(-3.,1.,10.6));
#7714=CARTESIAN_POINT('Origin',(0.,0.,10.6));
#7715=CARTESIAN_POINT('Origin',(0.,0.,10.6));
#7716=CARTESIAN_POINT('Origin',(0.,0.,10.6));
#7717=CARTESIAN_POINT('',(0.,0.,0.));
#7718=CARTESIAN_POINT('Origin',(1.75,0.,9.9));
#7719=CARTESIAN_POINT('',(2.09482142857143,0.14738786380825,10.4));
#7720=CARTESIAN_POINT('',(2.09482142857143,0.147387863808251,10.));
#7721=CARTESIAN_POINT('',(2.09482142857143,0.14738786380825,9.9));
#7722=CARTESIAN_POINT('',(2.09482142857143,-0.14738786380825,10.4));
#7723=CARTESIAN_POINT('Origin',(1.75,0.,10.4));
#7724=CARTESIAN_POINT('',(2.09482142857143,-0.147387863808251,10.));
#7725=CARTESIAN_POINT('',(2.09482142857143,-0.14738786380825,9.9));
#7726=CARTESIAN_POINT('Origin',(1.75,0.,10.));
#7727=CARTESIAN_POINT('Origin',(1.75,0.,10.4));
#7728=CARTESIAN_POINT('Origin',(0.,0.,10.4));
#7729=CARTESIAN_POINT('',(1.525,2.75545529808155E-17,10.4));
#7730=CARTESIAN_POINT('Origin',(1.75,0.,10.4));
#7731=CARTESIAN_POINT('Origin',(-0.875,1.51554445662277,9.9));
#7732=CARTESIAN_POINT('',(-1.17505234855318,1.74047464163074,10.4));
#7733=CARTESIAN_POINT('',(-1.17505234855318,1.74047464163074,10.));
#7734=CARTESIAN_POINT('',(-1.17505234855318,1.74047464163074,9.9));
#7735=CARTESIAN_POINT('',(-0.919769080018249,1.88786250543899,10.4));
#7736=CARTESIAN_POINT('Origin',(-0.875,1.51554445662277,10.4));
#7737=CARTESIAN_POINT('',(-0.919769080018247,1.88786250543899,10.));
#7738=CARTESIAN_POINT('',(-0.919769080018249,1.88786250543899,9.9));
#7739=CARTESIAN_POINT('Origin',(-0.875,1.51554445662277,10.));
#7740=CARTESIAN_POINT('Origin',(-0.875,1.51554445662277,10.4));
#7741=CARTESIAN_POINT('Origin',(0.,0.,10.4));
#7742=CARTESIAN_POINT('',(-1.1,1.51554445662277,10.4));
#7743=CARTESIAN_POINT('Origin',(-0.875,1.51554445662277,10.4));
#7744=CARTESIAN_POINT('Origin',(-0.875000000000001,-1.51554445662277,9.9));
#7745=CARTESIAN_POINT('',(-0.91976908001825,-1.88786250543899,10.4));
#7746=CARTESIAN_POINT('',(-0.919769080018249,-1.88786250543899,10.));
#7747=CARTESIAN_POINT('',(-0.91976908001825,-1.88786250543899,9.9));
#7748=CARTESIAN_POINT('',(-1.17505234855318,-1.74047464163074,10.4));
#7749=CARTESIAN_POINT('Origin',(-0.875000000000001,-1.51554445662277,10.4));
#7750=CARTESIAN_POINT('',(-1.17505234855318,-1.74047464163074,10.));
#7751=CARTESIAN_POINT('',(-1.17505234855318,-1.74047464163074,9.9));
#7752=CARTESIAN_POINT('Origin',(-0.875000000000001,-1.51554445662277,10.));
#7753=CARTESIAN_POINT('Origin',(-0.875000000000001,-1.51554445662277,10.4));
#7754=CARTESIAN_POINT('Origin',(0.,0.,10.4));
#7755=CARTESIAN_POINT('',(-1.1,-1.51554445662277,10.4));
#7756=CARTESIAN_POINT('Origin',(-0.875000000000001,-1.51554445662277,10.4));
#7757=CARTESIAN_POINT('Origin',(0.,0.,10.));
#7758=CARTESIAN_POINT('Origin',(0.,0.,10.));
#7759=CARTESIAN_POINT('',(-2.1,-2.57175827820944E-16,10.));
#7760=CARTESIAN_POINT('Origin',(0.,0.,10.));
#7761=CARTESIAN_POINT('Origin',(0.,0.,10.));
#7762=CARTESIAN_POINT('Origin',(0.,0.,10.));
#7763=CARTESIAN_POINT('',(-1.02,-1.2491397351303E-16,10.));
#7764=CARTESIAN_POINT('Origin',(0.,0.,10.));
#7765=CARTESIAN_POINT('Origin',(1.75,0.,9.9));
#7766=CARTESIAN_POINT('',(1.525,2.75545529808155E-17,10.6));
#7767=CARTESIAN_POINT('',(1.525,-2.75545529808155E-17,9.9));
#7768=CARTESIAN_POINT('Origin',(1.75,0.,10.6));
#7769=CARTESIAN_POINT('Origin',(-0.875,1.51554445662277,9.9));
#7770=CARTESIAN_POINT('',(-1.1,1.51554445662277,10.6));
#7771=CARTESIAN_POINT('',(-1.1,1.51554445662277,9.9));
#7772=CARTESIAN_POINT('Origin',(-0.875,1.51554445662277,10.6));
#7773=CARTESIAN_POINT('Origin',(-0.875000000000001,-1.51554445662277,9.9));
#7774=CARTESIAN_POINT('',(-1.1,-1.51554445662277,10.6));
#7775=CARTESIAN_POINT('',(-1.1,-1.51554445662277,9.9));
#7776=CARTESIAN_POINT('Origin',(-0.875000000000001,-1.51554445662277,10.6));
#7777=CARTESIAN_POINT('Origin',(0.,0.,10.));
#7778=CARTESIAN_POINT('',(-1.02,-1.2491397351303E-16,10.6));
#7779=CARTESIAN_POINT('Origin',(0.,0.,10.6));
#7780=CARTESIAN_POINT('',(-1.02,-1.2491397351303E-16,10.));
#7781=CARTESIAN_POINT('Origin',(0.,0.,10.));
#7782=CARTESIAN_POINT('',(-2.1,-2.57175827820944E-16,10.6));
#7783=CARTESIAN_POINT('Origin',(0.,0.,10.6));
#7784=CARTESIAN_POINT('',(-2.1,-2.57175827820944E-16,10.));
#7785=CARTESIAN_POINT('Origin',(0.,0.,10.6));
#7786=CARTESIAN_POINT('',(0.,0.,0.));
#7787=CARTESIAN_POINT('Origin',(0.,-4.1,7.2));
#7788=CARTESIAN_POINT('',(-0.31,-4.,7.2));
#7789=CARTESIAN_POINT('Origin',(0.,-4.,7.2));
#7790=CARTESIAN_POINT('',(-0.31,-2.35,7.2));
#7791=CARTESIAN_POINT('',(-0.31,-4.1,7.2));
#7792=CARTESIAN_POINT('Origin',(0.,-2.35,7.2));
#7793=CARTESIAN_POINT('Origin',(-3.,-3.5,8.));
#7794=CARTESIAN_POINT('',(-3.,-2.5,6.4));
#7795=CARTESIAN_POINT('',(-3.,-2.5,8.));
#7796=CARTESIAN_POINT('',(-3.,-2.5,7.6));
#7797=CARTESIAN_POINT('',(-3.,-1.5,6.4));
#7798=CARTESIAN_POINT('',(-3.,-3.5,6.4));
#7799=CARTESIAN_POINT('',(-3.,-1.5,8.));
#7800=CARTESIAN_POINT('',(-3.,-1.5,6.4));
#7801=CARTESIAN_POINT('',(-3.,-3.5,8.));
#7802=CARTESIAN_POINT('Origin',(-3.75,-1.5,7.2));
#7803=CARTESIAN_POINT('',(-4.5,-1.5,8.));
#7804=CARTESIAN_POINT('',(-3.,-1.5,8.));
#7805=CARTESIAN_POINT('',(-4.5,-1.5,6.4));
#7806=CARTESIAN_POINT('',(-4.5,-1.5,6.4));
#7807=CARTESIAN_POINT('',(-4.5,-1.5,8.));
#7808=CARTESIAN_POINT('Origin',(0.,-3.175,8.));
#7809=CARTESIAN_POINT('',(-0.8,-3.5,8.));
#7810=CARTESIAN_POINT('',(-4.5,-3.5,8.));
#7811=CARTESIAN_POINT('',(-0.8,-3.5,8.));
#7812=CARTESIAN_POINT('',(-0.8,-4.,8.));
#7813=CARTESIAN_POINT('',(-0.8,-2.35,8.));
#7814=CARTESIAN_POINT('',(0.8,-4.,8.));
#7815=CARTESIAN_POINT('',(-0.8,-4.,8.));
#7816=CARTESIAN_POINT('',(0.8,-2.35,8.));
#7817=CARTESIAN_POINT('',(0.8,-4.,8.));
#7818=CARTESIAN_POINT('',(-0.8,-2.35,8.));
#7819=CARTESIAN_POINT('',(0.8,-2.35,8.));
#7820=CARTESIAN_POINT('',(-0.8,-2.5,8.));
#7821=CARTESIAN_POINT('',(-0.8,-2.35,8.));
#7822=CARTESIAN_POINT('',(-0.8,-2.5,8.));
#7823=CARTESIAN_POINT('',(-4.5,-3.5,8.));
#7824=CARTESIAN_POINT('Origin',(-4.5,-3.5,6.4));
#7825=CARTESIAN_POINT('',(-4.5,-3.5,6.4));
#7826=CARTESIAN_POINT('',(-4.5,-3.5,8.));
#7827=CARTESIAN_POINT('',(-4.5,-3.5,6.4));
#7828=CARTESIAN_POINT('Origin',(-2.65,-2.5,7.2));
#7829=CARTESIAN_POINT('',(-0.8,-2.5,6.4));
#7830=CARTESIAN_POINT('',(-0.8,-2.5,6.8));
#7831=CARTESIAN_POINT('',(-4.5,-2.5,6.4));
#7832=CARTESIAN_POINT('Origin',(-2.65,-3.5,7.2));
#7833=CARTESIAN_POINT('',(-0.8,-3.5,6.4));
#7834=CARTESIAN_POINT('',(-4.5,-3.5,6.4));
#7835=CARTESIAN_POINT('',(-0.8,-3.5,6.8));
#7836=CARTESIAN_POINT('Origin',(-0.8,-2.35,6.4));
#7837=CARTESIAN_POINT('',(-0.8,-4.,6.4));
#7838=CARTESIAN_POINT('',(-0.8,-2.35,6.4));
#7839=CARTESIAN_POINT('',(-0.8,-4.,6.4));
#7840=CARTESIAN_POINT('Origin',(-0.8,-2.35,6.4));
#7841=CARTESIAN_POINT('',(-0.8,-2.35,6.4));
#7842=CARTESIAN_POINT('',(-0.8,-2.35,6.4));
#7843=CARTESIAN_POINT('',(-0.8,-2.35,6.4));
#7844=CARTESIAN_POINT('Origin',(0.8,-2.35,6.4));
#7845=CARTESIAN_POINT('',(0.8,-2.35,6.4));
#7846=CARTESIAN_POINT('',(0.8,-2.35,6.4));
#7847=CARTESIAN_POINT('',(0.8,-2.35,6.4));
#7848=CARTESIAN_POINT('Origin',(0.8,-4.,6.4));
#7849=CARTESIAN_POINT('',(0.8,-4.,6.4));
#7850=CARTESIAN_POINT('',(0.8,-4.,6.4));
#7851=CARTESIAN_POINT('',(0.8,-4.,6.4));
#7852=CARTESIAN_POINT('Origin',(-0.8,-4.,6.4));
#7853=CARTESIAN_POINT('',(-0.8,-4.,6.4));
#7854=CARTESIAN_POINT('Origin',(0.,-3.175,6.4));
#7855=CARTESIAN_POINT('',(0.,0.,0.));
#7856=CARTESIAN_POINT('Origin',(0.,-2.13,7.2));
#7857=CARTESIAN_POINT('',(-1.83697019872103E-17,-2.13,7.5));
#7858=CARTESIAN_POINT('',(-1.83697019872103E-17,-2.13,6.9));
#7859=CARTESIAN_POINT('Origin',(0.,-2.13,7.2));
#7860=CARTESIAN_POINT('',(0.,0.,0.));
#7861=CARTESIAN_POINT('Origin',(0.,-2.6,7.2));
#7862=CARTESIAN_POINT('',(-0.29,-2.6,7.2));
#7863=CARTESIAN_POINT('Origin',(0.,-2.6,7.2));
#7864=CARTESIAN_POINT('',(-0.1,-2.6,7.2));
#7865=CARTESIAN_POINT('Origin',(0.,-2.6,7.2));
#7866=CARTESIAN_POINT('Origin',(0.,-2.6,7.2));
#7867=CARTESIAN_POINT('',(-0.29,-2.43,7.2));
#7868=CARTESIAN_POINT('Origin',(0.,-2.43,7.2));
#7869=CARTESIAN_POINT('',(-0.29,-2.6,7.2));
#7870=CARTESIAN_POINT('Origin',(0.,-5.,7.2));
#7871=CARTESIAN_POINT('',(-0.1,-5.,7.2));
#7872=CARTESIAN_POINT('',(-0.1,-5.,7.2));
#7873=CARTESIAN_POINT('Origin',(0.,-5.,7.2));
#7874=CARTESIAN_POINT('Origin',(0.,-2.43,7.2));
#7875=CARTESIAN_POINT('Origin',(0.,-5.,7.2));
#7876=CARTESIAN_POINT('',(0.,0.,0.));
#7877=CARTESIAN_POINT('Origin',(0.,-4.,7.2));
#7878=CARTESIAN_POINT('',(-0.6,-4.,7.2));
#7879=CARTESIAN_POINT('Origin',(0.,-4.,7.2));
#7880=CARTESIAN_POINT('',(-0.31,-4.,7.2));
#7881=CARTESIAN_POINT('Origin',(0.,-4.,7.2));
#7882=CARTESIAN_POINT('Origin',(0.,-4.2,7.2));
#7883=CARTESIAN_POINT('',(-0.6,-4.2,7.2));
#7884=CARTESIAN_POINT('',(-0.6,-4.2,7.2));
#7885=CARTESIAN_POINT('Origin',(0.,-4.2,7.2));
#7886=CARTESIAN_POINT('Origin',(0.,-4.2,7.2));
#7887=CARTESIAN_POINT('',(-0.11,-4.2,7.2));
#7888=CARTESIAN_POINT('Origin',(0.,-4.2,7.2));
#7889=CARTESIAN_POINT('Origin',(0.,-4.,7.2));
#7890=CARTESIAN_POINT('',(-0.11,-3.6,7.2));
#7891=CARTESIAN_POINT('Origin',(0.,-3.6,7.2));
#7892=CARTESIAN_POINT('',(-0.11,-4.,7.2));
#7893=CARTESIAN_POINT('Origin',(0.,-4.,7.2));
#7894=CARTESIAN_POINT('',(-0.31,-3.6,7.2));
#7895=CARTESIAN_POINT('Origin',(0.,-3.6,7.2));
#7896=CARTESIAN_POINT('',(-0.31,-4.,7.2));
#7897=CARTESIAN_POINT('Origin',(0.,-3.6,7.2));
#7898=CARTESIAN_POINT('',(0.,0.,0.));
#7899=CARTESIAN_POINT('Origin',(0.,-5.,7.2));
#7900=CARTESIAN_POINT('',(-0.1,-4.6,7.2));
#7901=CARTESIAN_POINT('Origin',(0.,-4.6,7.2));
#7902=CARTESIAN_POINT('',(-0.1,-5.,7.2));
#7903=CARTESIAN_POINT('',(-0.1,-5.,7.2));
#7904=CARTESIAN_POINT('Origin',(0.,-5.,7.2));
#7905=CARTESIAN_POINT('Origin',(0.,-5.,7.2));
#7906=CARTESIAN_POINT('',(-0.6,-4.6,7.2));
#7907=CARTESIAN_POINT('Origin',(0.,-4.6,7.2));
#7908=CARTESIAN_POINT('',(-0.6,-5.,7.2));
#7909=CARTESIAN_POINT('',(-0.6,-5.,7.2));
#7910=CARTESIAN_POINT('Origin',(0.,-5.,7.2));
#7911=CARTESIAN_POINT('Origin',(0.,-4.6,7.2));
#7912=CARTESIAN_POINT('Origin',(0.,-5.,7.2));
#7913=CARTESIAN_POINT('',(0.,0.,0.));
#7914=CARTESIAN_POINT('Ctrl Pts',(0.199999521685004,-2.62021022067982,7.20354528529548));
#7915=CARTESIAN_POINT('Ctrl Pts',(0.19999343949118,-2.6255753643916,7.24862669087077));
#7916=CARTESIAN_POINT('Ctrl Pts',(0.168615691452697,-2.63634781999191,7.33868016798294));
#7917=CARTESIAN_POINT('Ctrl Pts',(0.0459616996448183,-2.65270477799173,
7.41618164971903));
#7918=CARTESIAN_POINT('Ctrl Pts',(-0.0998469869656992,-2.66924595959392,
7.39996507729611));
#7919=CARTESIAN_POINT('Ctrl Pts',(-0.204936181985623,-2.68597304189578,
7.29527847685269));
#7920=CARTESIAN_POINT('Ctrl Pts',(-0.221986969755699,-2.7028797483455,7.14628505326925));
#7921=CARTESIAN_POINT('Ctrl Pts',(-0.141631327334848,-2.71996166380803,
7.01788664502262));
#7922=CARTESIAN_POINT('Ctrl Pts',(0.00270481241442627,-2.73721192504324,
6.96708134679183));
#7923=CARTESIAN_POINT('Ctrl Pts',(0.143039113459417,-2.75397833948373,7.01603761180454));
#7924=CARTESIAN_POINT('Ctrl Pts',(0.223330027417085,-2.77023316539608,7.13370506584288));
#7925=CARTESIAN_POINT('Ctrl Pts',(0.223609433092684,-2.7859516486779,7.2713911725354));
#7926=CARTESIAN_POINT('Ctrl Pts',(0.152101468687107,-2.80045790761646,7.37648984952004));
#7927=CARTESIAN_POINT('Ctrl Pts',(0.0493840180807327,-2.81371750007274,
7.42583309513969));
#7928=CARTESIAN_POINT('Ctrl Pts',(-0.0535656424988985,-2.82570326133932,
7.42596307871198));
#7929=CARTESIAN_POINT('Ctrl Pts',(-0.146731811694293,-2.83773755003964,
7.38108373553243));
#7930=CARTESIAN_POINT('Ctrl Pts',(-0.211512387655128,-2.8498166397957,7.29998894076038));
#7931=CARTESIAN_POINT('Ctrl Pts',(-0.234672692510252,-2.86193666288461,
7.19851881716116));
#7932=CARTESIAN_POINT('Ctrl Pts',(-0.211502078818359,-2.87409363541626,
7.09651570260184));
#7933=CARTESIAN_POINT('Ctrl Pts',(-0.146175031667225,-2.88628349462379,
7.01496045942807));
#7934=CARTESIAN_POINT('Ctrl Pts',(-0.0201759406699065,-2.90257490033143,
6.95334279019282));
#7935=CARTESIAN_POINT('Ctrl Pts',(0.164048433167981,-2.92300029227989,6.99488705015939));
#7936=CARTESIAN_POINT('Ctrl Pts',(0.263212640482471,-2.94757377707087,7.20034626829039));
#7937=CARTESIAN_POINT('Ctrl Pts',(0.16413428164115,-2.9721746956776,7.40571604889496));
#7938=CARTESIAN_POINT('Ctrl Pts',(-0.0580809020736254,-2.99676718133414,
7.45651943873815));
#7939=CARTESIAN_POINT('Ctrl Pts',(-0.236127517621773,-3.02131545740765,
7.31427023254914));
#7940=CARTESIAN_POINT('Ctrl Pts',(-0.235623291843773,-3.04374517395574,
7.10674242176483));
#7941=CARTESIAN_POINT('Ctrl Pts',(-0.107269644782094,-3.06405280900675,
6.97972425972366));
#7942=CARTESIAN_POINT('Ctrl Pts',(0.0527757922260714,-3.08225163138773,
6.96159979137369));
#7943=CARTESIAN_POINT('Ctrl Pts',(0.188726377923501,-3.10035885514916,7.04734634676648));
#7944=CARTESIAN_POINT('Ctrl Pts',(0.232341637226282,-3.11536108595312,7.17289318656827));
#7945=CARTESIAN_POINT('Ctrl Pts',(0.215074929637344,-3.12730445561105,7.27290788199928));
#7946=CARTESIAN_POINT('Ctrl Pts',(0.166334604203376,-3.13920694864625,7.3615533699487));
#7947=CARTESIAN_POINT('Ctrl Pts',(0.0552567235661542,-3.1540048293497,7.43128948802867));
#7948=CARTESIAN_POINT('Ctrl Pts',(-0.100043793704833,-3.17162317434127,
7.4135433615447));
#7949=CARTESIAN_POINT('Ctrl Pts',(-0.209398878386583,-3.18909256344761,
7.30384381469642));
#7950=CARTESIAN_POINT('Ctrl Pts',(-0.226357160076232,-3.20640410002376,
7.15124619930781));
#7951=CARTESIAN_POINT('Ctrl Pts',(-0.145244888291477,-3.22354989628281,
7.02263774678675));
#7952=CARTESIAN_POINT('Ctrl Pts',(-0.00307739889558997,-3.24052311289208,
6.9731562179116));
#7953=CARTESIAN_POINT('Ctrl Pts',(0.137388780060693,-3.25731801286151,7.02262233145429));
#7954=CARTESIAN_POINT('Ctrl Pts',(0.215568012201749,-3.27392998789316,7.14745036721));
#7955=CARTESIAN_POINT('Ctrl Pts',(0.199056669422034,-3.29035561704227,7.29224338602279));
#7956=CARTESIAN_POINT('Ctrl Pts',(0.0972442378117871,-3.30659260084323,
7.39359267072072));
#7957=CARTESIAN_POINT('Ctrl Pts',(-0.0606078656788346,-3.32442299860284,
7.41159207397961));
#7958=CARTESIAN_POINT('Ctrl Pts',(-0.174349434794334,-3.34024917344643,
7.3202399790036));
#7959=CARTESIAN_POINT('Ctrl Pts',(-0.200242071600934,-3.35415023112003,
7.20325404432313));
#7960=CARTESIAN_POINT('Ctrl Pts',(-0.18063258547865,-3.36449358017806,7.11681410663695));
#7961=CARTESIAN_POINT('Ctrl Pts',(-0.125490051337177,-3.37475550369447,
7.04788845684967));
#7962=CARTESIAN_POINT('Ctrl Pts',(-0.0466957223057233,-3.38493729013136,
7.00998942647324));
#7963=CARTESIAN_POINT('Ctrl Pts',(0.0401186427931674,-3.39504044724382,
7.01009457046437));
#7964=CARTESIAN_POINT('Ctrl Pts',(0.117713403951327,-3.40506669595631,7.04749596858794));
#7965=CARTESIAN_POINT('Ctrl Pts',(0.170930387597076,-3.41501799177983,7.11440539415709));
#7966=CARTESIAN_POINT('Ctrl Pts',(0.18979238088286,-3.42489648282701,7.1971524208448));
#7967=CARTESIAN_POINT('Ctrl Pts',(0.17093827709221,-3.43470453492267,7.2792766512254));
#7968=CARTESIAN_POINT('Ctrl Pts',(0.123087817102158,-3.44363304446436,7.33923456804198));
#7969=CARTESIAN_POINT('Ctrl Pts',(0.0630389653927127,-3.45170235370222,
7.37229315652779));
#7970=CARTESIAN_POINT('Ctrl Pts',(-0.0177036729288225,-3.46133839204526,
7.38615351281265));
#7971=CARTESIAN_POINT('Ctrl Pts',(-0.11772305137169,-3.47329787855213,7.35109019812551));
#7972=CARTESIAN_POINT('Ctrl Pts',(-0.184714685581635,-3.48752403008714,
7.24410703240861));
#7973=CARTESIAN_POINT('Ctrl Pts',(-0.17053859750796,-3.50163575663314,7.11977423357787));
#7974=CARTESIAN_POINT('Ctrl Pts',(-0.082587996452088,-3.51564730527911,
7.03201669890537));
#7975=CARTESIAN_POINT('Ctrl Pts',(0.0401074098738201,-3.52956782204744,
7.0182572369454));
#7976=CARTESIAN_POINT('Ctrl Pts',(0.144033604536224,-3.54341977713357,7.08377705773452));
#7977=CARTESIAN_POINT('Ctrl Pts',(0.170884312908661,-3.55260377562906,7.16051919899628));
#7978=CARTESIAN_POINT('Ctrl Pts',(0.170889524395514,-3.55720086923049,7.1991469511116));
#7979=CARTESIAN_POINT('Ctrl Pts',(0.191023542756439,-2.62021022067982,7.20354407429412));
#7980=CARTESIAN_POINT('Ctrl Pts',(0.191017726414002,-2.62534085511048,7.24665498129917));
#7981=CARTESIAN_POINT('Ctrl Pts',(0.161033850394857,-2.63563485658156,7.33273947644214));
#7982=CARTESIAN_POINT('Ctrl Pts',(0.0436799375629447,-2.6512854138931,7.40693000436112));
#7983=CARTESIAN_POINT('Ctrl Pts',(-0.0959987808218971,-2.66712696375714,
7.39142052099388));
#7984=CARTESIAN_POINT('Ctrl Pts',(-0.196829905250034,-2.68316922567495,
7.29102743103875));
#7985=CARTESIAN_POINT('Ctrl Pts',(-0.213252255362172,-2.69940855979398,
7.14788433221334));
#7986=CARTESIAN_POINT('Ctrl Pts',(-0.135952056419508,-2.71584543096616,
7.0242793563294));
#7987=CARTESIAN_POINT('Ctrl Pts',(0.00322439729343584,-2.73247671681477,
6.97523297281595));
#7988=CARTESIAN_POINT('Ctrl Pts',(0.138869091438245,-2.74867593022619,7.02249383745227));
#7989=CARTESIAN_POINT('Ctrl Pts',(0.216674071017294,-2.76441519194789,7.13643570930967));
#7990=CARTESIAN_POINT('Ctrl Pts',(0.216990443986426,-2.77967065524482,7.27008142439094));
#7991=CARTESIAN_POINT('Ctrl Pts',(0.147461738971512,-2.79377910905693,7.37235184002062));
#7992=CARTESIAN_POINT('Ctrl Pts',(0.047333450735047,-2.80670380678563,7.42047652131588));
#7993=CARTESIAN_POINT('Ctrl Pts',(-0.0532106536911018,-2.81840737559959,
7.4206256558615));
#7994=CARTESIAN_POINT('Ctrl Pts',(-0.144378744511407,-2.83018047137138,
7.37673185790055));
#7995=CARTESIAN_POINT('Ctrl Pts',(-0.207902064816201,-2.84201938593495,
7.29724909461857));
#7996=CARTESIAN_POINT('Ctrl Pts',(-0.230670002371674,-2.85392183859013,
7.19758944399363));
#7997=CARTESIAN_POINT('Ctrl Pts',(-0.207893335338729,-2.86588164249669,
7.0972028957719));
#7998=CARTESIAN_POINT('Ctrl Pts',(-0.143487364744061,-2.87790004133283,
7.01676930123252));
#7999=CARTESIAN_POINT('Ctrl Pts',(-0.0190193226663081,-2.89399389208917,
6.95585884391441));
#8000=CARTESIAN_POINT('Ctrl Pts',(0.163586328894419,-2.91422968067412,6.99687105352309));
#8001=CARTESIAN_POINT('Ctrl Pts',(0.262456471900163,-2.9386767814229,7.20122686982788));
#8002=CARTESIAN_POINT('Ctrl Pts',(0.16364689697854,-2.96325138569098,7.40652598693401));
#8003=CARTESIAN_POINT('Ctrl Pts',(-0.059251333627089,-2.98791913148238,
7.45770124310656));
#8004=CARTESIAN_POINT('Ctrl Pts',(-0.238744875888964,-3.01264249790562,
7.31456854455266));
#8005=CARTESIAN_POINT('Ctrl Pts',(-0.238414861081409,-3.03532370670177,
7.1046723413934));
#8006=CARTESIAN_POINT('Ctrl Pts',(-0.108219790599525,-3.05592692071135,
6.97569591466389));
#8007=CARTESIAN_POINT('Ctrl Pts',(0.0546507861677333,-3.07444227191367,
6.95717854257545));
#8008=CARTESIAN_POINT('Ctrl Pts',(0.193437408460763,-3.09291982793468,7.04462472677658));
#8009=CARTESIAN_POINT('Ctrl Pts',(0.238122848764674,-3.10826703109889,7.17307568347903));
#8010=CARTESIAN_POINT('Ctrl Pts',(0.220429833499831,-3.12051104548578,7.2756216678726));
#8011=CARTESIAN_POINT('Ctrl Pts',(0.170406454940412,-3.13272858443559,7.36662390053473));
#8012=CARTESIAN_POINT('Ctrl Pts',(0.056200071240455,-3.14794419657849,7.43838646727187));
#8013=CARTESIAN_POINT('Ctrl Pts',(-0.103895504850653,-3.16610350899751,
7.42015451305419));
#8014=CARTESIAN_POINT('Ctrl Pts',(-0.216908103553831,-3.18414862458417,
7.30686416228629));
#8015=CARTESIAN_POINT('Ctrl Pts',(-0.234513691775253,-3.20206759837303,
7.14890287443755));
#8016=CARTESIAN_POINT('Ctrl Pts',(-0.150429627901186,-3.2198483950201,7.01549612364992));
#8017=CARTESIAN_POINT('Ctrl Pts',(-0.00275052944868849,-3.23748023207103,
6.96405310813854));
#8018=CARTESIAN_POINT('Ctrl Pts',(0.143402720749719,-3.2549531655216,7.01548469083049));
#8019=CARTESIAN_POINT('Ctrl Pts',(0.224869691209636,-3.27225819798112,7.14550628408959));
#8020=CARTESIAN_POINT('Ctrl Pts',(0.207674446226838,-3.2893875862004,7.2965024724066));
#8021=CARTESIAN_POINT('Ctrl Pts',(0.101426890655383,-3.30633493427357,7.40228966269414));
#8022=CARTESIAN_POINT('Ctrl Pts',(-0.0634150898376773,-3.32495614129161,
7.4210979000742));
#8023=CARTESIAN_POINT('Ctrl Pts',(-0.1822359591826,-3.34149060327876,7.32567014640293));
#8024=CARTESIAN_POINT('Ctrl Pts',(-0.209280485902103,-3.35601236711325,
7.20346528253749));
#8025=CARTESIAN_POINT('Ctrl Pts',(-0.188795825646846,-3.36681636246986,
7.11318643013913));
#8026=CARTESIAN_POINT('Ctrl Pts',(-0.131216307204934,-3.37753199733383,
7.04122143073785));
#8027=CARTESIAN_POINT('Ctrl Pts',(-0.048975801731852,-3.3881599612999,7.00167277093901));
#8028=CARTESIAN_POINT('Ctrl Pts',(0.0415822516777477,-3.39869985613274,
7.00178871033236));
#8029=CARTESIAN_POINT('Ctrl Pts',(0.122464106224022,-3.40915267810657,7.04078440402212));
#8030=CARTESIAN_POINT('Ctrl Pts',(0.177886120551665,-3.41951877896738,7.11047882697577));
#8031=CARTESIAN_POINT('Ctrl Pts',(0.197502916828992,-3.42979927641084,7.19658381053113));
#8032=CARTESIAN_POINT('Ctrl Pts',(0.177896449457243,-3.43999561916638,7.28194224811453));
#8033=CARTESIAN_POINT('Ctrl Pts',(0.128212743394908,-3.44926556361253,7.34417843697285));
#8034=CARTESIAN_POINT('Ctrl Pts',(0.0659471883228922,-3.45763455664724,
7.37845138672491));
#8035=CARTESIAN_POINT('Ctrl Pts',(-0.0176843848898256,-3.46761643973737,
7.39279899859123));
#8036=CARTESIAN_POINT('Ctrl Pts',(-0.121083708756642,-3.47998778018346,
7.35650173270899));
#8037=CARTESIAN_POINT('Ctrl Pts',(-0.190111930497616,-3.49466307862108,
7.24614193421259));
#8038=CARTESIAN_POINT('Ctrl Pts',(-0.175463764144624,-3.50917928747668,
7.11830222206023));
#8039=CARTESIAN_POINT('Ctrl Pts',(-0.0852554106795787,-3.52354649168734,
7.02839732944465));
#8040=CARTESIAN_POINT('Ctrl Pts',(0.0401061072486938,-3.53777296100086,
7.01441443337408));
#8041=CARTESIAN_POINT('Ctrl Pts',(0.145858454765231,-3.55187732457476,7.0811740864261));
#8042=CARTESIAN_POINT('Ctrl Pts',(0.17305380815376,-3.56119542074233,7.1590096425235));
#8043=CARTESIAN_POINT('Ctrl Pts',(0.173059084396458,-3.56584963598494,7.19811736759295));
#8044=CARTESIAN_POINT('Ctrl Pts',(0.173158501738058,-2.62873184854516,7.20252750402056));
#8045=CARTESIAN_POINT('Ctrl Pts',(0.173153218829459,-2.63339193743202,7.2416845831989));
#8046=CARTESIAN_POINT('Ctrl Pts',(0.145938970756177,-2.64272474633487,7.31968447296958));
#8047=CARTESIAN_POINT('Ctrl Pts',(0.0397348763892528,-2.65689026062815,
7.38679369226741));
#8048=CARTESIAN_POINT('Ctrl Pts',(-0.0864890400134375,-2.67120973124552,
7.37274979393911));
#8049=CARTESIAN_POINT('Ctrl Pts',(-0.177560438111068,-2.68570416834132,
7.28207185920492));
#8050=CARTESIAN_POINT('Ctrl Pts',(-0.192407596533418,-2.70037922212494,
7.15275928313263));
#8051=CARTESIAN_POINT('Ctrl Pts',(-0.122540417469413,-2.71524574150998,
7.0409920671935));
#8052=CARTESIAN_POINT('Ctrl Pts',(0.00346341303810412,-2.73031050711819,
6.99654562940632));
#8053=CARTESIAN_POINT('Ctrl Pts',(0.126554930146189,-2.74501481989148,7.03938106158892));
#8054=CARTESIAN_POINT('Ctrl Pts',(0.197363865868405,-2.75933707765723,7.14299597376079));
#8055=CARTESIAN_POINT('Ctrl Pts',(0.197704056060021,-2.77325401319431,7.26489099146508));
#8056=CARTESIAN_POINT('Ctrl Pts',(0.134130381062669,-2.786168336898,7.35849624306076));
#8057=CARTESIAN_POINT('Ctrl Pts',(0.0422460255745021,-2.79803276136078,
7.40269519912191));
#8058=CARTESIAN_POINT('Ctrl Pts',(-0.0502919619965319,-2.8088075022445,
7.40285907057282));
#8059=CARTESIAN_POINT('Ctrl Pts',(-0.134469523268098,-2.81967842050119,
7.36236888554382));
#8060=CARTESIAN_POINT('Ctrl Pts',(-0.193322485979024,-2.83064537823505,
7.28878115409414));
#8061=CARTESIAN_POINT('Ctrl Pts',(-0.214513633921132,-2.84170727748237,
7.19618893172989));
#8062=CARTESIAN_POINT('Ctrl Pts',(-0.193316277704633,-2.85286429839084,
7.10257534531843));
#8063=CARTESIAN_POINT('Ctrl Pts',(-0.133070873823438,-2.86411323797119,
7.0272822312058));
#8064=CARTESIAN_POINT('Ctrl Pts',(-0.0162062490412889,-2.87923391733063,
6.97002261633703));
#8065=CARTESIAN_POINT('Ctrl Pts',(0.156368886155166,-2.89836026042033,7.00846997516318));
#8066=CARTESIAN_POINT('Ctrl Pts',(0.250905090253854,-2.9216527068464,7.20291604024908));
#8067=CARTESIAN_POINT('Ctrl Pts',(0.156382586273267,-2.94526590871319,7.40029658879584));
#8068=CARTESIAN_POINT('Ctrl Pts',(-0.0594801303014584,-2.96917467862821,
7.45031261861394));
#8069=CARTESIAN_POINT('Ctrl Pts',(-0.235239905615142,-2.99335132894538,
7.31075364916488));
#8070=CARTESIAN_POINT('Ctrl Pts',(-0.235324261158338,-3.01572980435851,
7.10370529224427));
#8071=CARTESIAN_POINT('Ctrl Pts',(-0.10602170037884,-3.03622281987395,6.9752854815943));
#8072=CARTESIAN_POINT('Ctrl Pts',(0.0570006024249987,-3.05476604528251,
6.95657099108577));
#8073=CARTESIAN_POINT('Ctrl Pts',(0.196978986837661,-3.07339085238332,7.04453594814324));
#8074=CARTESIAN_POINT('Ctrl Pts',(0.242467752552828,-3.08896870185106,7.1748237890863));
#8075=CARTESIAN_POINT('Ctrl Pts',(0.224455215333573,-3.10145518627921,7.27939935476355));
#8076=CARTESIAN_POINT('Ctrl Pts',(0.17331013027485,-3.11395563571474,7.37250667012694));
#8077=CARTESIAN_POINT('Ctrl Pts',(0.0559775593867093,-3.12960297019709,
7.44641139018859));
#8078=CARTESIAN_POINT('Ctrl Pts',(-0.109693476081705,-3.14839546460465,
7.42772920012961));
#8079=CARTESIAN_POINT('Ctrl Pts',(-0.227486258030471,-3.16718695551515,
7.30989707575346));
#8080=CARTESIAN_POINT('Ctrl Pts',(-0.246098856844244,-3.18595987633661,
7.14444836244404));
#8081=CARTESIAN_POINT('Ctrl Pts',(-0.157640602442323,-3.2046971614539,7.00379198862032));
#8082=CARTESIAN_POINT('Ctrl Pts',(-0.00120601544693738,-3.22338180286804,
6.9491324800669));
#8083=CARTESIAN_POINT('Ctrl Pts',(0.154546474484069,-3.24199717653129,7.00378599134579));
#8084=CARTESIAN_POINT('Ctrl Pts',(0.241897815202096,-3.26052712642461,7.14293476115058));
#8085=CARTESIAN_POINT('Ctrl Pts',(0.223524906976926,-3.27895597756738,7.30540511372487));
#8086=CARTESIAN_POINT('Ctrl Pts',(0.108790492948344,-3.29726854793425,7.41980440638438));
#8087=CARTESIAN_POINT('Ctrl Pts',(-0.0700533440103121,-3.31747119125551,
7.44034864847014));
#8088=CARTESIAN_POINT('Ctrl Pts',(-0.199623057501188,-3.33548579374738,
7.33648540438074));
#8089=CARTESIAN_POINT('Ctrl Pts',(-0.229221414974038,-3.35135671295434,
7.20291396417937));
#8090=CARTESIAN_POINT('Ctrl Pts',(-0.206809680372079,-3.36318519045383,
7.10405847819106));
#8091=CARTESIAN_POINT('Ctrl Pts',(-0.143675377283367,-3.37493610128364,
7.02511964802601));
#8092=CARTESIAN_POINT('Ctrl Pts',(-0.0533626365384458,-3.38660622159859,
6.98167021818281));
#8093=CARTESIAN_POINT('Ctrl Pts',(0.046205156976151,-3.39819313055781,6.98178625579333));
#8094=CARTESIAN_POINT('Ctrl Pts',(0.135218488600369,-3.40969412427728,7.02469031539363));
#8095=CARTESIAN_POINT('Ctrl Pts',(0.196251716945606,-3.42110716597797,7.10143474403484));
#8096=CARTESIAN_POINT('Ctrl Pts',(0.217865285391825,-3.4324301939502,7.1962892325178));
#8097=CARTESIAN_POINT('Ctrl Pts',(0.196260535910131,-3.44366140556578,7.29033280776571));
#8098=CARTESIAN_POINT('Ctrl Pts',(0.141526130922779,-3.45387157509335,7.35889127434652));
#8099=CARTESIAN_POINT('Ctrl Pts',(0.0729583886246232,-3.4630842452824,7.39662788506617));
#8100=CARTESIAN_POINT('Ctrl Pts',(-0.0190940690797755,-3.47406867882678,
7.41241609379824));
#8101=CARTESIAN_POINT('Ctrl Pts',(-0.132779160970955,-3.48766247485799,
7.37247540729533));
#8102=CARTESIAN_POINT('Ctrl Pts',(-0.208489105531237,-3.50375946110311,
7.25133738069355));
#8103=CARTESIAN_POINT('Ctrl Pts',(-0.192394326071967,-3.519638321504,7.11142720311936));
#8104=CARTESIAN_POINT('Ctrl Pts',(-0.0939403593005316,-3.53530277168423,
7.01341338007167));
#8105=CARTESIAN_POINT('Ctrl Pts',(0.0422605125078274,-3.55075075526385,
6.99832278160776));
#8106=CARTESIAN_POINT('Ctrl Pts',(0.1565440859987,-3.56599599233585,7.07060828215171));
#8107=CARTESIAN_POINT('Ctrl Pts',(0.185698876792587,-3.57601155541678,7.15436510947656));
#8108=CARTESIAN_POINT('Ctrl Pts',(0.185704536106873,-3.58100368112599,7.19631217672005));
#8109=CARTESIAN_POINT('Ctrl Pts',(0.166525366620545,-2.65758658420228,7.19909260340903));
#8110=CARTESIAN_POINT('Ctrl Pts',(0.166520289008348,-2.66206557976378,7.23672801940631));
#8111=CARTESIAN_POINT('Ctrl Pts',(0.140348275753376,-2.67098879281991,7.31126270005341));
#8112=CARTESIAN_POINT('Ctrl Pts',(0.0399774791194812,-2.68435583849075,
7.37438039593517));
#8113=CARTESIAN_POINT('Ctrl Pts',(-0.0776574996962614,-2.69770347508532,
7.36105620850106));
#8114=CARTESIAN_POINT('Ctrl Pts',(-0.161408766434036,-2.71105687135119,
7.27734776640516));
#8115=CARTESIAN_POINT('Ctrl Pts',(-0.174728238572193,-2.72442979432405,
7.15947416895345));
#8116=CARTESIAN_POINT('Ctrl Pts',(-0.111526458500605,-2.73784095508408,
7.05873826484987));
#8117=CARTESIAN_POINT('Ctrl Pts',(0.00117829704477278,-2.75130656740219,
7.01917259019172));
#8118=CARTESIAN_POINT('Ctrl Pts',(0.11026863481546,-2.7643421103719,7.05729331555389));
#8119=CARTESIAN_POINT('Ctrl Pts',(0.172542463585331,-2.77695269446299,7.14859557088421));
#8120=CARTESIAN_POINT('Ctrl Pts',(0.172758419267171,-2.78913933013576,7.25534594832492));
#8121=CARTESIAN_POINT('Ctrl Pts',(0.117297375174102,-2.80039298929176,7.33689338067046));
#8122=CARTESIAN_POINT('Ctrl Pts',(0.0374793460091744,-2.81069732757045,
7.37525827577019));
#8123=CARTESIAN_POINT('Ctrl Pts',(-0.0426999334578007,-2.82003179746841,
7.37538143917469));
#8124=CARTESIAN_POINT('Ctrl Pts',(-0.115480105067975,-2.82943089377101,
7.34035492146379));
#8125=CARTESIAN_POINT('Ctrl Pts',(-0.166283399534618,-2.8388982290778,7.2768148162638));
#8126=CARTESIAN_POINT('Ctrl Pts',(-0.184550847892414,-2.84843746708543,
7.19695788907849));
#8127=CARTESIAN_POINT('Ctrl Pts',(-0.166278739115269,-2.85805148397594,
7.11627641094483));
#8128=CARTESIAN_POINT('Ctrl Pts',(-0.11436157509869,-2.86774415878459,7.05139195278408));
#8129=CARTESIAN_POINT('Ctrl Pts',(-0.0136373605432596,-2.88077580648601,
7.00203726516335));
#8130=CARTESIAN_POINT('Ctrl Pts',(0.135270491135525,-2.8972745142599,7.03513970278866));
#8131=CARTESIAN_POINT('Ctrl Pts',(0.217212305752653,-2.91742718851122,7.20332132024231));
#8132=CARTESIAN_POINT('Ctrl Pts',(0.135257996783122,-2.93794808980581,7.37497192443284));
#8133=CARTESIAN_POINT('Ctrl Pts',(-0.0533876532778471,-2.9588476861815,
7.41897307812886));
#8134=CARTESIAN_POINT('Ctrl Pts',(-0.208357363305794,-2.98013180670875,
7.29637221500731));
#8135=CARTESIAN_POINT('Ctrl Pts',(-0.208783521385516,-2.99999644346923,
7.1125597718962));
#8136=CARTESIAN_POINT('Ctrl Pts',(-0.0932051793686978,-3.01833445242994,
6.99745969229246));
#8137=CARTESIAN_POINT('Ctrl Pts',(0.0537644028633427,-3.03505132869382,
6.98040447259593));
#8138=CARTESIAN_POINT('Ctrl Pts',(0.181096825444236,-3.05197751615123,7.06017345938295));
#8139=CARTESIAN_POINT('Ctrl Pts',(0.222956282771945,-3.06625169664934,7.17952184368757));
#8140=CARTESIAN_POINT('Ctrl Pts',(0.206375060569474,-3.07776961978831,7.27600523510941));
#8141=CARTESIAN_POINT('Ctrl Pts',(0.159022777496631,-3.08935174812889,7.36228595692239));
#8142=CARTESIAN_POINT('Ctrl Pts',(0.049676708892268,-3.10394701180979,7.43139250849058));
#8143=CARTESIAN_POINT('Ctrl Pts',(-0.106345964297192,-3.12164088568468,
7.41405454588476));
#8144=CARTESIAN_POINT('Ctrl Pts',(-0.218508477592453,-3.13950380517162,
7.30222030391762));
#8145=CARTESIAN_POINT('Ctrl Pts',(-0.236640596317295,-3.15752444745288,
7.14342530883726));
#8146=CARTESIAN_POINT('Ctrl Pts',(-0.151108234377237,-3.17569037824872,
7.00690875886963));
#8147=CARTESIAN_POINT('Ctrl Pts',(0.0020000497825991,-3.19398828187494,
6.95311663906165));
#8148=CARTESIAN_POINT('Ctrl Pts',(0.156175162605377,-3.2124039849716,7.00692181511878));
#8149=CARTESIAN_POINT('Ctrl Pts',(0.243712267918876,-3.23092257241902,7.14582938427287));
#8150=CARTESIAN_POINT('Ctrl Pts',(0.225444644405621,-3.24952839182458,7.30988852205161));
#8151=CARTESIAN_POINT('Ctrl Pts',(0.1086266700814,-3.26820558032915,7.42674224413357));
#8152=CARTESIAN_POINT('Ctrl Pts',(-0.0755568103276177,-3.28901857118917,
7.44826275819282));
#8153=CARTESIAN_POINT('Ctrl Pts',(-0.210876101071928,-3.30779418668607,
7.34037569434887));
#8154=CARTESIAN_POINT('Ctrl Pts',(-0.242158837615405,-3.32449655055692,
7.19981012826506));
#8155=CARTESIAN_POINT('Ctrl Pts',(-0.218482747686626,-3.33702480679517,
7.09510428287159));
#8156=CARTESIAN_POINT('Ctrl Pts',(-0.151258418917599,-3.349549304472,7.01092210100317));
#8157=CARTESIAN_POINT('Ctrl Pts',(-0.0544388795806348,-3.36206501623859,
6.96426376579124));
#8158=CARTESIAN_POINT('Ctrl Pts',(0.0529848938244735,-3.37456676113353,
6.96431686779002));
#8159=CARTESIAN_POINT('Ctrl Pts',(0.149618681042139,-3.38704954076379,7.0108168542326));
#8160=CARTESIAN_POINT('Ctrl Pts',(0.216294125348177,-3.39950831444022,7.09454634215613));
#8161=CARTESIAN_POINT('Ctrl Pts',(0.240082283609214,-3.41193813883908,7.19864862883354));
#8162=CARTESIAN_POINT('Ctrl Pts',(0.216301417199454,-3.42433422652378,7.30245308275509));
#8163=CARTESIAN_POINT('Ctrl Pts',(0.155624789134382,-3.43566184662336,7.37854450982395));
#8164=CARTESIAN_POINT('Ctrl Pts',(0.0792338751048572,-3.44592835125056,
7.42061757097289));
#8165=CARTESIAN_POINT('Ctrl Pts',(-0.0236947435290427,-3.45821303575049,
7.43830643547426));
#8166=CARTESIAN_POINT('Ctrl Pts',(-0.1515457831225,-3.47349927012097,7.39355105926792));
#8167=CARTESIAN_POINT('Ctrl Pts',(-0.237353326682969,-3.49171555422899,
7.25657816758057));
#8168=CARTESIAN_POINT('Ctrl Pts',(-0.219180338240666,-3.50979141387795,
7.09733539274298));
#8169=CARTESIAN_POINT('Ctrl Pts',(-0.106639336531097,-3.52771395650611,
6.98511360449985));
#8170=CARTESIAN_POINT('Ctrl Pts',(0.049865171992709,-3.54547134962642,6.96768469168436));
#8171=CARTESIAN_POINT('Ctrl Pts',(0.181721726166896,-3.56305313157731,7.05095143559938));
#8172=CARTESIAN_POINT('Ctrl Pts',(0.215498137389901,-3.57464974765708,7.14788703905096));
#8173=CARTESIAN_POINT('Ctrl Pts',(0.215504679516594,-3.58042060914303,7.19637754768492));
#8174=CARTESIAN_POINT('Ctrl Pts',(0.185107472272675,-2.68073719173477,7.19633995373285));
#8175=CARTESIAN_POINT('Ctrl Pts',(0.185101850763769,-2.68569596220842,7.23800674867565));
#8176=CARTESIAN_POINT('Ctrl Pts',(0.156058199319024,-2.69556022858565,7.32034333803071));
#8177=CARTESIAN_POINT('Ctrl Pts',(0.0462369377041908,-2.71016597633029,
7.38909331331611));
#8178=CARTESIAN_POINT('Ctrl Pts',(-0.0808600379235311,-2.72459415027127,
7.37446486049346));
#8179=CARTESIAN_POINT('Ctrl Pts',(-0.170106237630621,-2.73885403619876,
7.28488979381794));
#8180=CARTESIAN_POINT('Ctrl Pts',(-0.183880616709954,-2.75295769295724,
7.16056856294843));
#8181=CARTESIAN_POINT('Ctrl Pts',(-0.117863262566178,-2.76691743614216,
7.05587052443364));
#8182=CARTESIAN_POINT('Ctrl Pts',(-0.0020314316850335,-2.7807468107492,
7.01551272108977));
#8183=CARTESIAN_POINT('Ctrl Pts',(0.10837582499231,-2.79395216768506,7.05438162297723));
#8184=CARTESIAN_POINT('Ctrl Pts',(0.170462788399269,-2.80656117379754,7.14577794914887));
#8185=CARTESIAN_POINT('Ctrl Pts',(0.170483716515046,-2.818596730844,7.25120669361347));
#8186=CARTESIAN_POINT('Ctrl Pts',(0.11623013408604,-2.82957663370843,7.33066673575509));
#8187=CARTESIAN_POINT('Ctrl Pts',(0.0391429351448043,-2.83952479252818,
7.36762207289601));
#8188=CARTESIAN_POINT('Ctrl Pts',(-0.0375831622377559,-2.84845722206348,
7.36766609159734));
#8189=CARTESIAN_POINT('Ctrl Pts',(-0.106590866905911,-2.85737386804714,
7.33437242450682));
#8190=CARTESIAN_POINT('Ctrl Pts',(-0.154323772729316,-2.86627970238647,
7.27455761393419));
#8191=CARTESIAN_POINT('Ctrl Pts',(-0.171301646699268,-2.87517996511473,
7.20003709996095));
#8192=CARTESIAN_POINT('Ctrl Pts',(-0.154317119566702,-2.88407962497398,
7.1253713308374));
#8193=CARTESIAN_POINT('Ctrl Pts',(-0.106586603192965,-2.89298402606097,
7.06580203076649));
#8194=CARTESIAN_POINT('Ctrl Pts',(-0.0146581859250508,-2.9048694987715,
7.02086680405053));
#8195=CARTESIAN_POINT('Ctrl Pts',(0.119679747928827,-2.91976334307369,7.05112432742094));
#8196=CARTESIAN_POINT('Ctrl Pts',(0.192359619789719,-2.9377356556885,7.20129666148723));
#8197=CARTESIAN_POINT('Ctrl Pts',(0.119710574570271,-2.95584663711404,7.35261634156035));
#8198=CARTESIAN_POINT('Ctrl Pts',(-0.0454133776145315,-2.97413387650899,
7.39082897056735));
#8199=CARTESIAN_POINT('Ctrl Pts',(-0.179953115079168,-2.99263280954147,
7.28410167764536));
#8200=CARTESIAN_POINT('Ctrl Pts',(-0.180187116386609,-3.00981476342207,
7.12511842248155));
#8201=CARTESIAN_POINT('Ctrl Pts',(-0.080455868059763,-3.02563503905427,
7.02585734601489));
#8202=CARTESIAN_POINT('Ctrl Pts',(0.0461874797537591,-3.04003938796267,
7.01117283714634));
#8203=CARTESIAN_POINT('Ctrl Pts',(0.155889163671215,-3.05462162210191,7.07988905593192));
#8204=CARTESIAN_POINT('Ctrl Pts',(0.192002101108853,-3.06692816231653,7.18278090837932));
#8205=CARTESIAN_POINT('Ctrl Pts',(0.177695431363444,-3.07687134320315,7.26607724746195));
#8206=CARTESIAN_POINT('Ctrl Pts',(0.136780671630806,-3.08688063865225,7.34064380608613));
#8207=CARTESIAN_POINT('Ctrl Pts',(0.0421316192783748,-3.0995177452559,7.40052761266016));
#8208=CARTESIAN_POINT('Ctrl Pts',(-0.0934338623745871,-3.11489020621722,
7.38555268889591));
#8209=CARTESIAN_POINT('Ctrl Pts',(-0.191368949641329,-3.13047459530452,
7.28805591492407));
#8210=CARTESIAN_POINT('Ctrl Pts',(-0.207391636243208,-3.1462741944362,7.14884163693624));
#8211=CARTESIAN_POINT('Ctrl Pts',(-0.132098549251811,-3.16229064327564,
7.02839785341959));
#8212=CARTESIAN_POINT('Ctrl Pts',(0.00369007158893442,-3.17852431513169,
6.98052015501029));
#8213=CARTESIAN_POINT('Ctrl Pts',(0.14147140548659,-3.19497417066394,7.02842015914195));
#8214=CARTESIAN_POINT('Ctrl Pts',(0.220404755355712,-3.21163773974047,7.1533143737985));
#8215=CARTESIAN_POINT('Ctrl Pts',(0.204040148119795,-3.22851185815579,7.30213076349379));
#8216=CARTESIAN_POINT('Ctrl Pts',(0.0973630617653471,-3.24559011238179,
7.40912719498989));
#8217=CARTESIAN_POINT('Ctrl Pts',(-0.0724753624674162,-3.26478678833049,
7.42926923462765));
#8218=CARTESIAN_POINT('Ctrl Pts',(-0.198857150771922,-3.28228664005936,
7.32901755401093));
#8219=CARTESIAN_POINT('Ctrl Pts',(-0.228415618223813,-3.29800120150021,
7.19676443740428));
#8220=CARTESIAN_POINT('Ctrl Pts',(-0.206056653052093,-3.30986343736228,
7.09761156829177));
#8221=CARTESIAN_POINT('Ctrl Pts',(-0.142055048123301,-3.32179879095291,
7.01733731331786));
#8222=CARTESIAN_POINT('Ctrl Pts',(-0.0492154972805245,-3.33380382681927,
6.9725138159443));
#8223=CARTESIAN_POINT('Ctrl Pts',(0.0545114782345651,-3.34587484328919,
6.97248829472171));
#8224=CARTESIAN_POINT('Ctrl Pts',(0.148474547415015,-3.35800808352178,7.01761622718362));
#8225=CARTESIAN_POINT('Ctrl Pts',(0.213783582718699,-3.37019943651325,7.09950448341927));
#8226=CARTESIAN_POINT('Ctrl Pts',(0.237296599865736,-3.38244484532487,7.20204554953723));
#8227=CARTESIAN_POINT('Ctrl Pts',(0.213786034721385,-3.39473983718185,7.30502757685629));
#8228=CARTESIAN_POINT('Ctrl Pts',(0.153251203560767,-3.40605176457476,7.38106061938234));
#8229=CARTESIAN_POINT('Ctrl Pts',(0.0765239927439651,-3.41636484949048,
7.42336069496949));
#8230=CARTESIAN_POINT('Ctrl Pts',(-0.0273847389731562,-3.42876839128249,
7.44126747332444));
#8231=CARTESIAN_POINT('Ctrl Pts',(-0.157533033535677,-3.44431985844659,
7.3959554283747));
#8232=CARTESIAN_POINT('Ctrl Pts',(-0.245963473728323,-3.46304035049211,
7.25534056816814));
#8233=CARTESIAN_POINT('Ctrl Pts',(-0.227377089922609,-3.48180333014707,
7.09001457354066));
#8234=CARTESIAN_POINT('Ctrl Pts',(-0.10959705092368,-3.50059017332273,6.9721779507632));
#8235=CARTESIAN_POINT('Ctrl Pts',(0.0560250788067464,-3.51938704187467,
6.95348154924594));
#8236=CARTESIAN_POINT('Ctrl Pts',(0.197052436429245,-3.53816884599807,7.04220437160198));
#8237=CARTESIAN_POINT('Ctrl Pts',(0.233628963287126,-3.55068088369041,7.14674488416437));
#8238=CARTESIAN_POINT('Ctrl Pts',(0.233636036508055,-3.55692022758386,7.19917188482486));
#8239=CARTESIAN_POINT('Ctrl Pts',(0.214878329241221,-2.68071167631188,7.19634700688545));
#8240=CARTESIAN_POINT('Ctrl Pts',(0.21487182329556,-2.68645061434203,7.24456927394994));
#8241=CARTESIAN_POINT('Ctrl Pts',(0.181215095804958,-2.69789401566424,7.34010917676144));
#8242=CARTESIAN_POINT('Ctrl Pts',(0.0537659785169842,-2.71484126590492,
7.41988663023413));
#8243=CARTESIAN_POINT('Ctrl Pts',(-0.09373371851528,-2.73158585390756,7.40290940748877));
#8244=CARTESIAN_POINT('Ctrl Pts',(-0.197166167452985,-2.74811534933935,
7.29903046327851));
#8245=CARTESIAN_POINT('Ctrl Pts',(-0.213034321110582,-2.76443051525134,
7.15519994000744));
#8246=CARTESIAN_POINT('Ctrl Pts',(-0.136819975557523,-2.78052820707376,
7.03450142161169));
#8247=CARTESIAN_POINT('Ctrl Pts',(-0.00375351882357425,-2.79640902509429,
6.98826242279056));
#8248=CARTESIAN_POINT('Ctrl Pts',(0.122333193616463,-2.81149365697418,7.03278955833157));
#8249=CARTESIAN_POINT('Ctrl Pts',(0.192744669714971,-2.82581172202087,7.13664478499631));
#8250=CARTESIAN_POINT('Ctrl Pts',(0.192647881053207,-2.8393914952052,7.25560741643829));
#8251=CARTESIAN_POINT('Ctrl Pts',(0.131770645966198,-2.85169082997991,7.34455022261805));
#8252=CARTESIAN_POINT('Ctrl Pts',(0.0459939732724772,-2.86275697963967,
7.3855948352218));
#8253=CARTESIAN_POINT('Ctrl Pts',(-0.0388130362826423,-2.87262995943921,
7.38558203095042));
#8254=CARTESIAN_POINT('Ctrl Pts',(-0.114539127899638,-2.88241859001702,
7.34897184256002));
#8255=CARTESIAN_POINT('Ctrl Pts',(-0.166511534095061,-2.89212570551886,
7.28373270044754));
#8256=CARTESIAN_POINT('Ctrl Pts',(-0.184810079874889,-2.90175391362293,
7.20310188788887));
#8257=CARTESIAN_POINT('Ctrl Pts',(-0.166499070669721,-2.91130664969882,
7.12297856836614));
#8258=CARTESIAN_POINT('Ctrl Pts',(-0.115640722633783,-2.92078670707761,
7.05960552710051));
#8259=CARTESIAN_POINT('Ctrl Pts',(-0.0185035951711087,-2.93333502747441,
7.01225906285182));
#8260=CARTESIAN_POINT('Ctrl Pts',(0.121384202754409,-2.94885754279125,7.04432810744503));
#8261=CARTESIAN_POINT('Ctrl Pts',(0.195134680693374,-2.96725491613172,7.19836545333501));
#8262=CARTESIAN_POINT('Ctrl Pts',(0.121492212412953,-2.98545720090378,7.35011748851036));
#8263=CARTESIAN_POINT('Ctrl Pts',(-0.0415756095516308,-3.00350071291157,
7.38713785532324));
#8264=CARTESIAN_POINT('Ctrl Pts',(-0.171471644948999,-3.02142390268615,
7.28320999930232));
#8265=CARTESIAN_POINT('Ctrl Pts',(-0.171122013040012,-3.03777918677307,
7.1319049638478));
#8266=CARTESIAN_POINT('Ctrl Pts',(-0.0773985344224403,-3.05261903400135,
7.039049711749));
#8267=CARTESIAN_POINT('Ctrl Pts',(0.0399833773515873,-3.06597019341009,
7.02566105807932));
#8268=CARTESIAN_POINT('Ctrl Pts',(0.140369924424537,-3.07933150614831,7.08880680890486));
#8269=CARTESIAN_POINT('Ctrl Pts',(0.172952186649219,-3.09049185762763,7.18213910205967));
#8270=CARTESIAN_POINT('Ctrl Pts',(0.160047639831177,-3.09944207648492,7.2570980192185));
#8271=CARTESIAN_POINT('Ctrl Pts',(0.123360578173005,-3.10841052070708,7.32389555825651));
#8272=CARTESIAN_POINT('Ctrl Pts',(0.0390364069690545,-3.11966187978331,
7.37708457574868));
#8273=CARTESIAN_POINT('Ctrl Pts',(-0.0806839027680721,-3.13324221912812,
7.36370840776829));
#8274=CARTESIAN_POINT('Ctrl Pts',(-0.166516225814016,-3.14691808423354,
7.27808190977155));
#8275=CARTESIAN_POINT('Ctrl Pts',(-0.1803885024237,-3.16070433204962,7.15662107539426));
#8276=CARTESIAN_POINT('Ctrl Pts',(-0.114933495650407,-3.17461568751952,
7.05207571305458));
#8277=CARTESIAN_POINT('Ctrl Pts',(0.00258664962602312,-3.18866585403527,
7.01070631425415));
#8278=CARTESIAN_POINT('Ctrl Pts',(0.121500437060258,-3.20286770222029,7.05209149218014));
#8279=CARTESIAN_POINT('Ctrl Pts',(0.189515967342179,-3.21723327862761,7.15974852768408));
#8280=CARTESIAN_POINT('Ctrl Pts',(0.175418084641306,-3.2317720828774,7.2879569750776));
#8281=CARTESIAN_POINT('Ctrl Pts',(0.0834767702888784,-3.24649681310668,
7.38019750575045));
#8282=CARTESIAN_POINT('Ctrl Pts',(-0.063118475428651,-3.26307103030429,
7.39764002158794));
#8283=CARTESIAN_POINT('Ctrl Pts',(-0.172586769126297,-3.27822107611759,
7.31094414714426));
#8284=CARTESIAN_POINT('Ctrl Pts',(-0.198306357495174,-3.29187213671086,
7.19607145757355));
#8285=CARTESIAN_POINT('Ctrl Pts',(-0.178855476148038,-3.30220421737521,
7.10971022421916));
#8286=CARTESIAN_POINT('Ctrl Pts',(-0.122973787180029,-3.31263115861789,
7.03956593295181));
#8287=CARTESIAN_POINT('Ctrl Pts',(-0.041619423464239,-3.32315369917206,
7.00024936303785));
#8288=CARTESIAN_POINT('Ctrl Pts',(0.0496224608427707,-3.33377249093432,
7.0001876752484));
#8289=CARTESIAN_POINT('Ctrl Pts',(0.132615977620369,-3.34448764766654,7.04000114288187));
#8290=CARTESIAN_POINT('Ctrl Pts',(0.190567079631117,-3.35529935310258,7.11259019946977));
#8291=CARTESIAN_POINT('Ctrl Pts',(0.211557095963147,-3.36620709548451,7.20391423560445));
#8292=CARTESIAN_POINT('Ctrl Pts',(0.19056766958691,-3.3772106311537,7.29608667824698));
#8293=CARTESIAN_POINT('Ctrl Pts',(0.136166978738086,-3.38738386597841,7.36449481817329));
#8294=CARTESIAN_POINT('Ctrl Pts',(0.0668637166489791,-3.39670087321399,
7.40273214763341));
#8295=CARTESIAN_POINT('Ctrl Pts',(-0.0273632555059043,-3.40795054895204,
7.41900543577496));
#8296=CARTESIAN_POINT('Ctrl Pts',(-0.146177376821207,-3.42214234210721,
7.37782632931633));
#8297=CARTESIAN_POINT('Ctrl Pts',(-0.227756280424957,-3.43937189049888,
7.24854197729575));
#8298=CARTESIAN_POINT('Ctrl Pts',(-0.210735924661904,-3.45679498612433,
7.09500736118589));
#8299=CARTESIAN_POINT('Ctrl Pts',(-0.100539622313171,-3.4744007837155,6.98440854237947));
#8300=CARTESIAN_POINT('Ctrl Pts',(0.0561077229205953,-3.49218430227486,
6.96647422873777));
#8301=CARTESIAN_POINT('Ctrl Pts',(0.190963235128123,-3.51012426777635,7.05099318661589));
#8302=CARTESIAN_POINT('Ctrl Pts',(0.226408417556183,-3.5221978574293,7.15180919947803));
#8303=CARTESIAN_POINT('Ctrl Pts',(0.226415268139349,-3.52824081079723,7.20258599999129));
#8304=CARTESIAN_POINT('Ctrl Pts',(0.233538303779023,-2.65759637264774,7.19910047958883));
#8305=CARTESIAN_POINT('Ctrl Pts',(0.23353123930546,-2.66382799186311,7.25146257244798));
#8306=CARTESIAN_POINT('Ctrl Pts',(0.19696745884569,-2.6763073269123,7.3556708689899));
#8307=CARTESIAN_POINT('Ctrl Pts',(0.0569730084398323,-2.69494130883234,
7.44356718383999));
#8308=CARTESIAN_POINT('Ctrl Pts',(-0.106524442685284,-2.71350166413368,
7.42496929134948));
#8309=CARTESIAN_POINT('Ctrl Pts',(-0.222163571737669,-2.73196121008211,
7.3091230299507));
#8310=CARTESIAN_POINT('Ctrl Pts',(-0.240199522465172,-2.75030982448797,
7.14741578501388));
#8311=CARTESIAN_POINT('Ctrl Pts',(-0.154095608050911,-2.76853080499078,
7.01072914726199));
#8312=CARTESIAN_POINT('Ctrl Pts',(-0.00267460687807611,-2.78661147066547,
6.95794871950724));
#8313=CARTESIAN_POINT('Ctrl Pts',(0.14164030899789,-2.8038747511127,7.00878148038353));
#8314=CARTESIAN_POINT('Ctrl Pts',(0.222615117792197,-2.82032946000645,7.12807539253736));
#8315=CARTESIAN_POINT('Ctrl Pts',(0.222566032265283,-2.83598692966601,7.26523101242083));
#8316=CARTESIAN_POINT('Ctrl Pts',(0.152222724280741,-2.85020730425676,7.36808448669668));
#8317=CARTESIAN_POINT('Ctrl Pts',(0.052883269474769,-2.86302436513278,7.41563755649051));
#8318=CARTESIAN_POINT('Ctrl Pts',(-0.0454508997787033,-2.87447229970568,
7.41563379936155));
#8319=CARTESIAN_POINT('Ctrl Pts',(-0.133324971812771,-2.88583102579193,
7.37315841026056));
#8320=CARTESIAN_POINT('Ctrl Pts',(-0.193653504241113,-2.89709830105743,
7.29743342327476));
#8321=CARTESIAN_POINT('Ctrl Pts',(-0.214889368558948,-2.90827301861113,
7.20385133456187));
#8322=CARTESIAN_POINT('Ctrl Pts',(-0.193640662373467,-2.91935338080873,
7.11091006412822));
#8323=CARTESIAN_POINT('Ctrl Pts',(-0.134699243008982,-2.93033890052561,
7.03748141089585));
#8324=CARTESIAN_POINT('Ctrl Pts',(-0.0222774827983604,-2.94485821758379,
6.98270915909811));
#8325=CARTESIAN_POINT('Ctrl Pts',(0.139091593640502,-2.96276591757136,7.01987612520336));
#8326=CARTESIAN_POINT('Ctrl Pts',(0.223437037797074,-2.98386877798849,7.196730445542));
#8327=CARTESIAN_POINT('Ctrl Pts',(0.139257378147977,-3.00458867914989,7.36934332497687));
#8328=CARTESIAN_POINT('Ctrl Pts',(-0.0447572277219394,-3.02493383754544,
7.41066476064657));
#8329=CARTESIAN_POINT('Ctrl Pts',(-0.189286778967101,-3.04491624179778,
7.29436254156531));
#8330=CARTESIAN_POINT('Ctrl Pts',(-0.188403825735976,-3.06291651894871,
7.12780952218904));
#8331=CARTESIAN_POINT('Ctrl Pts',(-0.0863353928960517,-3.07904135259068,
7.02711014487625));
#8332=CARTESIAN_POINT('Ctrl Pts',(0.0398108006740648,-3.09337910804554,
7.01296405421245));
#8333=CARTESIAN_POINT('Ctrl Pts',(0.146208508440029,-3.10755812551401,7.08021718201157));
#8334=CARTESIAN_POINT('Ctrl Pts',(0.180131861009168,-3.11924556686056,7.17807435840992));
#8335=CARTESIAN_POINT('Ctrl Pts',(0.16670128029989,-3.12852929709267,7.25582324597245));
#8336=CARTESIAN_POINT('Ctrl Pts',(0.128849181526771,-3.1377695627669,7.32464682833912));
#8337=CARTESIAN_POINT('Ctrl Pts',(0.0427116800450749,-3.149239893477,7.37870702037907));
#8338=CARTESIAN_POINT('Ctrl Pts',(-0.0777006583769931,-3.16289693813138,
7.36496356140122));
#8339=CARTESIAN_POINT('Ctrl Pts',(-0.162663216489806,-3.17646003764126,
7.27980557815832));
#8340=CARTESIAN_POINT('Ctrl Pts',(-0.175962341940663,-3.18994594112167,
7.16090735254292));
#8341=CARTESIAN_POINT('Ctrl Pts',(-0.112537351249249,-3.20337070954953,
7.0601179958768));
#8342=CARTESIAN_POINT('Ctrl Pts',(-0.000481216033886487,-3.21675127677844,
7.02095151118088));
#8343=CARTESIAN_POINT('Ctrl Pts',(0.111296697656111,-3.23010475115374,7.06011758513708));
#8344=CARTESIAN_POINT('Ctrl Pts',(0.174298843579563,-3.24344811181235,7.16029176874159));
#8345=CARTESIAN_POINT('Ctrl Pts',(0.161127262848427,-3.25680162593276,7.27804919975625));
#8346=CARTESIAN_POINT('Ctrl Pts',(0.0774244337848529,-3.27017623909351,
7.36174389935327));
#8347=CARTESIAN_POINT('Ctrl Pts',(-0.0545258475331624,-3.28508517972487,
7.3771987766231));
#8348=CARTESIAN_POINT('Ctrl Pts',(-0.151842439762883,-3.2985726274777,7.29977278923544));
#8349=CARTESIAN_POINT('Ctrl Pts',(-0.174497392547656,-3.31063449086272,
7.19825771524167));
#8350=CARTESIAN_POINT('Ctrl Pts',(-0.157357750943022,-3.31972130199921,
7.12229297679189));
#8351=CARTESIAN_POINT('Ctrl Pts',(-0.108376416413373,-3.32885327484438,
7.06087320694589));
#8352=CARTESIAN_POINT('Ctrl Pts',(-0.0373643947482642,-3.33803498700604,
7.02658711572428));
#8353=CARTESIAN_POINT('Ctrl Pts',(0.0420064034120988,-3.34727056328954,
7.02656190673972));
#8354=CARTESIAN_POINT('Ctrl Pts',(0.113992645451419,-3.35656453452081,7.06112022321622));
#8355=CARTESIAN_POINT('Ctrl Pts',(0.164133070511383,-3.36592049244828,7.12395812004847));
#8356=CARTESIAN_POINT('Ctrl Pts',(0.182252226692838,-3.37534284388788,7.20285791598277));
#8357=CARTESIAN_POINT('Ctrl Pts',(0.164132253563985,-3.3848345376368,7.28237529070212));
#8358=CARTESIAN_POINT('Ctrl Pts',(0.117236828749836,-3.39360290117376,7.34133619710266));
#8359=CARTESIAN_POINT('Ctrl Pts',(0.0575242319280615,-3.40162933393007,
7.37427980345525));
#8360=CARTESIAN_POINT('Ctrl Pts',(-0.0236535488582548,-3.41132057199507,
7.38829815085827));
#8361=CARTESIAN_POINT('Ctrl Pts',(-0.126036636133201,-3.42354719842553,
7.35282484173021));
#8362=CARTESIAN_POINT('Ctrl Pts',(-0.196447507190014,-3.43841077228126,
7.24130556418034));
#8363=CARTESIAN_POINT('Ctrl Pts',(-0.181786690767014,-3.45347315019531,
7.10855232056132));
#8364=CARTESIAN_POINT('Ctrl Pts',(-0.0862766704206619,-3.46874015439278,
7.0125916034523));
#8365=CARTESIAN_POINT('Ctrl Pts',(0.0500732682335706,-3.48421890261266,
6.99687835328418));
#8366=CARTESIAN_POINT('Ctrl Pts',(0.168070534236532,-3.49990825557829,7.07070558821891));
#8367=CARTESIAN_POINT('Ctrl Pts',(0.199310683862651,-3.51051845488447,7.15928045848644));
#8368=CARTESIAN_POINT('Ctrl Pts',(0.199316725929205,-3.5158482093806,7.20406450104937));
#8369=CARTESIAN_POINT('Ctrl Pts',(0.226807069374228,-2.62874525353582,7.20253314673028));
#8370=CARTESIAN_POINT('Ctrl Pts',(0.226800193170563,-2.63481079862087,7.25349977739365));
#8371=CARTESIAN_POINT('Ctrl Pts',(0.191272485389705,-2.64698867836095,7.35528689274925));
#8372=CARTESIAN_POINT('Ctrl Pts',(0.0533110857492899,-2.66537236048706,
7.44226188191812));
#8373=CARTESIAN_POINT('Ctrl Pts',(-0.109667876964825,-2.68386464624667,
7.42398792365078));
#8374=CARTESIAN_POINT('Ctrl Pts',(-0.226294478669585,-2.70244725643931,
7.30754504264378));
#8375=CARTESIAN_POINT('Ctrl Pts',(-0.244914583118051,-2.72110552668272,
7.14309248345841));
#8376=CARTESIAN_POINT('Ctrl Pts',(-0.15668266949549,-2.73982241025182,7.00250636322875));
#8377=CARTESIAN_POINT('Ctrl Pts',(0.000360275167344028,-2.75858136287757,
6.94746740129157));
#8378=CARTESIAN_POINT('Ctrl Pts',(0.151688784472103,-2.77666942058048,7.00049231569798));
#8379=CARTESIAN_POINT('Ctrl Pts',(0.23748865440538,-2.79406856806348,7.12654303181867));
#8380=CARTESIAN_POINT('Ctrl Pts',(0.23761695716689,-2.81076579754878,7.27280866250993));
#8381=CARTESIAN_POINT('Ctrl Pts',(0.162117527595802,-2.82605484913246,7.38348851179891));
#8382=CARTESIAN_POINT('Ctrl Pts',(0.0545882621468924,-2.83993173646103,
7.43504994553777));
#8383=CARTESIAN_POINT('Ctrl Pts',(-0.0524979360585502,-2.85239907298462,
7.43511222101232));
#8384=CARTESIAN_POINT('Ctrl Pts',(-0.148769496310483,-2.86483915988807,
7.38865172607033));
#8385=CARTESIAN_POINT('Ctrl Pts',(-0.215254024761476,-2.87724759240759,
7.30530082688861));
#8386=CARTESIAN_POINT('Ctrl Pts',(-0.238821796662854,-2.88961903583731,
7.20171142411695));
#8387=CARTESIAN_POINT('Ctrl Pts',(-0.215238237798196,-2.90194974810172,
7.09827776484272));
#8388=CARTESIAN_POINT('Ctrl Pts',(-0.149364834601404,-2.91423378360337,
7.01614108176756));
#8389=CARTESIAN_POINT('Ctrl Pts',(-0.0231308706748203,-2.93054559789587,
6.95454388888739));
#8390=CARTESIAN_POINT('Ctrl Pts',(0.159420173978833,-2.95079940372033,6.99624966262056));
#8391=CARTESIAN_POINT('Ctrl Pts',(0.255873437394368,-2.97485199097034,7.19763372613105));
#8392=CARTESIAN_POINT('Ctrl Pts',(0.15957313095635,-2.99862366344323,7.39576846719451));
#8393=CARTESIAN_POINT('Ctrl Pts',(-0.0525587099637037,-3.02208750782865,
7.44363039833475));
#8394=CARTESIAN_POINT('Ctrl Pts',(-0.219931950941677,-3.04522091566892,
7.30913177612171));
#8395=CARTESIAN_POINT('Ctrl Pts',(-0.218965218054516,-3.06610519788919,
7.11593913699533));
#8396=CARTESIAN_POINT('Ctrl Pts',(-0.100501511682712,-3.08482617518605,
6.99907504856024));
#8397=CARTESIAN_POINT('Ctrl Pts',(0.0458164463407195,-3.10146601073649,
6.98269678592085));
#8398=CARTESIAN_POINT('Ctrl Pts',(0.168999497221885,-3.11788828933047,7.06061891332887));
#8399=CARTESIAN_POINT('Ctrl Pts',(0.208122474292555,-3.13139648646481,7.17367059053374));
#8400=CARTESIAN_POINT('Ctrl Pts',(0.192637292346469,-3.14209220126933,7.26321724442717));
#8401=CARTESIAN_POINT('Ctrl Pts',(0.149112713706763,-3.15271566117018,7.34232079626982));
#8402=CARTESIAN_POINT('Ctrl Pts',(0.0503918987656031,-3.16586237028332,
7.40415778281572));
#8403=CARTESIAN_POINT('Ctrl Pts',(-0.0867200805671385,-3.18142249838002,
7.38835737794119));
#8404=CARTESIAN_POINT('Ctrl Pts',(-0.182700211691555,-3.19677179886155,
7.29191823673));
#8405=CARTESIAN_POINT('Ctrl Pts',(-0.197437125539796,-3.21191412401389,
7.1584636059683));
#8406=CARTESIAN_POINT('Ctrl Pts',(-0.126707005483683,-3.22685574481417,
7.04645677722269));
#8407=CARTESIAN_POINT('Ctrl Pts',(-0.00319094454791707,-3.24160375982955,
7.00352504192919));
#8408=CARTESIAN_POINT('Ctrl Pts',(0.11856508268551,-3.25616661068809,7.04643998602982));
#8409=CARTESIAN_POINT('Ctrl Pts',(0.186244643735728,-3.270554152578,7.15453132429662));
#8410=CARTESIAN_POINT('Ctrl Pts',(0.171956140631049,-3.28477480105648,7.27987318903316));
#8411=CARTESIAN_POINT('Ctrl Pts',(0.083770472898142,-3.29884525026963,7.36768722105074));
#8412=CARTESIAN_POINT('Ctrl Pts',(-0.0531987671053138,-3.31432198686421,
7.3833677722724));
#8413=CARTESIAN_POINT('Ctrl Pts',(-0.152299260177419,-3.32810268380143,
7.3039248465455));
#8414=CARTESIAN_POINT('Ctrl Pts',(-0.174981847078137,-3.34025604687833,
7.20166189370968));
#8415=CARTESIAN_POINT('Ctrl Pts',(-0.157808289885975,-3.34932803257825,
7.12584849313869));
#8416=CARTESIAN_POINT('Ctrl Pts',(-0.109299772760072,-3.35836163086098,
7.06515673754344));
#8417=CARTESIAN_POINT('Ctrl Pts',(-0.0396742128789388,-3.36736140818118,
7.03162683559205));
#8418=CARTESIAN_POINT('Ctrl Pts',(0.0374060865469686,-3.37633248399835,
7.03167814263163));
#8419=CARTESIAN_POINT('Ctrl Pts',(0.106662131123058,-3.38527943925005,7.06501065247445));
#8420=CARTESIAN_POINT('Ctrl Pts',(0.154443458609935,-3.39420766474773,7.12500716832091));
#8421=CARTESIAN_POINT('Ctrl Pts',(0.171513122490573,-3.40312176328236,7.19966018133591));
#8422=CARTESIAN_POINT('Ctrl Pts',(0.154448810128273,-3.4120273277969,7.27423689345863));
#8423=CARTESIAN_POINT('Ctrl Pts',(0.110761145556717,-3.42018708551772,7.32906401524711));
#8424=CARTESIAN_POINT('Ctrl Pts',(0.0555624170066066,-3.42760636575424,
7.35948454642012));
#8425=CARTESIAN_POINT('Ctrl Pts',(-0.0190556043401421,-3.43651328476221,
7.37233115593073));
#8426=CARTESIAN_POINT('Ctrl Pts',(-0.112331457345363,-3.44766009018625,
7.33983175331251));
#8427=CARTESIAN_POINT('Ctrl Pts',(-0.175704040546785,-3.46107387540665,
7.23909310909943));
#8428=CARTESIAN_POINT('Ctrl Pts',(-0.162425909441732,-3.47454209114925,
7.12040978273045));
#8429=CARTESIAN_POINT('Ctrl Pts',(-0.0776194368412568,-3.48808204867214,
7.03542354959143));
#8430=CARTESIAN_POINT('Ctrl Pts',(0.0424348764358349,-3.50170807079122,
7.02170483465243));
#8431=CARTESIAN_POINT('Ctrl Pts',(0.145618410675924,-3.51543992220036,7.08642673131801));
#8432=CARTESIAN_POINT('Ctrl Pts',(0.172745123919546,-3.52466866031849,7.16348700295488));
#8433=CARTESIAN_POINT('Ctrl Pts',(0.172750382832977,-3.5293075892768,7.20246628278216));
#8434=CARTESIAN_POINT('Ctrl Pts',(0.208975500613569,-2.62021022067982,7.20354649629684));
#8435=CARTESIAN_POINT('Ctrl Pts',(0.208969152515337,-2.62580992044147,7.25059879342368));
#8436=CARTESIAN_POINT('Ctrl Pts',(0.176200542181115,-2.63705663059552,7.34462698401245));
#8437=CARTESIAN_POINT('Ctrl Pts',(0.0482380022249738,-2.65411768985976,
7.42545084377329));
#8438=CARTESIAN_POINT('Ctrl Pts',(-0.103720983462279,-2.67135555018703,
7.40853032917249));
#8439=CARTESIAN_POINT('Ctrl Pts',(-0.213091232946899,-2.68876552670636,
7.29953341464567));
#8440=CARTESIAN_POINT('Ctrl Pts',(-0.230778210290289,-2.70633773804461,
7.14465406518129));
#8441=CARTESIAN_POINT('Ctrl Pts',(-0.147346836969467,-2.7240630897452,7.01142232753577));
#8442=CARTESIAN_POINT('Ctrl Pts',(0.00219669286606783,-2.74193073856756,
6.95883670315601));
#8443=CARTESIAN_POINT('Ctrl Pts',(0.147274876105101,-2.75926262337493,7.00950168746689));
#8444=CARTESIAN_POINT('Ctrl Pts',(0.230088843486711,-2.77603178187632,7.13094085128893));
#8445=CARTESIAN_POINT('Ctrl Pts',(0.230334378766964,-2.7922170622316,7.2727313032445));
#8446=CARTESIAN_POINT('Ctrl Pts',(0.156818756385348,-2.80712034812938,7.3807101094845));
#8447=CARTESIAN_POINT('Ctrl Pts',(0.0514599371458473,-2.82071832270221,
7.4312969017612));
#8448=CARTESIAN_POINT('Ctrl Pts',(-0.053949273106916,-2.83298814079633,
7.43141235157773));
#8449=CARTESIAN_POINT('Ctrl Pts',(-0.149162803673346,-2.84528639082816,
7.38552243933886));
#8450=CARTESIAN_POINT('Ctrl Pts',(-0.215239756886203,-2.85760759853358,
7.30277372032405));
#8451=CARTESIAN_POINT('Ctrl Pts',(-0.238803777980285,-2.8699484285224,7.19943437440153));
#8452=CARTESIAN_POINT('Ctrl Pts',(-0.215229520115252,-2.88230106367663,
7.09576020758005));
#8453=CARTESIAN_POINT('Ctrl Pts',(-0.148939420593191,-2.89466611719909,
7.01303450291724));
#8454=CARTESIAN_POINT('Ctrl Pts',(-0.0213325673406164,-2.91115883006794,
6.95066970086975));
#8455=CARTESIAN_POINT('Ctrl Pts',(0.164620027801451,-2.93177219578512,6.99277194403154));
#8456=CARTESIAN_POINT('Ctrl Pts',(0.264140345441926,-2.95647425946544,7.1994621312341));
#8457=CARTESIAN_POINT('Ctrl Pts',(0.164728852326112,-2.98110257359385,7.4050323399217));
#8458=CARTESIAN_POINT('Ctrl Pts',(-0.0569443318317078,-3.0056223317769,
7.45549377665849));
#8459=CARTESIAN_POINT('Ctrl Pts',(-0.233655234082383,-3.02999749647669,
7.31403792989835));
#8460=CARTESIAN_POINT('Ctrl Pts',(-0.232974963582391,-3.05218001599301,
7.10874779894472));
#8461=CARTESIAN_POINT('Ctrl Pts',(-0.106388781594654,-3.07219040709644,
6.98361852003422));
#8462=CARTESIAN_POINT('Ctrl Pts',(0.0509166303138672,-3.09006797134932,
6.96587840747777));
#8463=CARTESIAN_POINT('Ctrl Pts',(0.184107855620212,-3.10781070899736,7.049980356836));
#8464=CARTESIAN_POINT('Ctrl Pts',(0.22667112837476,-3.12246458039756,7.17268484719045));
#8465=CARTESIAN_POINT('Ctrl Pts',(0.209820378030098,-3.13411078817146,7.27022208122515));
#8466=CARTESIAN_POINT('Ctrl Pts',(0.162337133022933,-3.14570167635411,7.35655665500323));
#8467=CARTESIAN_POINT('Ctrl Pts',(0.0543381183921439,-3.16007989039251,
7.42429494476246));
#8468=CARTESIAN_POINT('Ctrl Pts',(-0.0962325781952025,-3.17715803206852,
7.40702433836543));
#8469=CARTESIAN_POINT('Ctrl Pts',(-0.201968741853417,-3.19405130244851,
7.30086969204493));
#8470=CARTESIAN_POINT('Ctrl Pts',(-0.218281002748809,-3.21075559415295,
7.15358183271638));
#8471=CARTESIAN_POINT('Ctrl Pts',(-0.140111375872412,-3.22726635027305,
7.02973402788688));
#8472=CARTESIAN_POINT('Ctrl Pts',(-0.0034165106286539,-3.24358092971903,
6.98220471253357));
#8473=CARTESIAN_POINT('Ctrl Pts',(0.131391629234701,-3.25969776110748,7.02971930828623));
#8474=CARTESIAN_POINT('Ctrl Pts',(0.206292361264499,-3.27561627696566,7.14937558433617));
#8475=CARTESIAN_POINT('Ctrl Pts',(0.190461110925075,-3.29133937308174,7.2879807743595));
#8476=CARTESIAN_POINT('Ctrl Pts',(0.0930770533573671,-3.30686565126976,
7.38489251842631));
#8477=CARTESIAN_POINT('Ctrl Pts',(-0.0577831284559989,-3.32390509058752,
7.40207685645854));
#8478=CARTESIAN_POINT('Ctrl Pts',(-0.166431009430519,-3.33902296977876,
7.31480305950528));
#8479=CARTESIAN_POINT('Ctrl Pts',(-0.191165405660558,-3.35230195988059,
7.20305195896223));
#8480=CARTESIAN_POINT('Ctrl Pts',(-0.172430795699987,-3.36218424465458,
7.12046761230825));
#8481=CARTESIAN_POINT('Ctrl Pts',(-0.119735198215102,-3.37199121037803,
7.05459706635593));
#8482=CARTESIAN_POINT('Ctrl Pts',(-0.0444046399914078,-3.3817262001077,
7.01836103206837));
#8483=CARTESIAN_POINT('Ctrl Pts',(0.0386419326090535,-3.39139119363884,
7.0184564545768));
#8484=CARTESIAN_POINT('Ctrl Pts',(0.1129237126287,-3.40098989064185,7.05425452293928));
#8485=CARTESIAN_POINT('Ctrl Pts',(0.163917462051814,-3.41052478524528,7.11835470673475));
#8486=CARTESIAN_POINT('Ctrl Pts',(0.182015951489857,-3.41999969889282,7.19771033519379));
#8487=CARTESIAN_POINT('Ctrl Pts',(0.163925204547397,-3.42941792680988,7.27656408688283));
#8488=CARTESIAN_POINT('Ctrl Pts',(0.117932620661441,-3.43800234053243,7.33421196773936));
#8489=CARTESIAN_POINT('Ctrl Pts',(0.0601344625788096,-3.44577115500963,
7.36603928463948));
#8490=CARTESIAN_POINT('Ctrl Pts',(-0.017670556131189,-3.45505825853875,
7.3794035026531));
#8491=CARTESIAN_POINT('Ctrl Pts',(-0.114246172587839,-3.46660968997134,
7.34559229118226));
#8492=CARTESIAN_POINT('Ctrl Pts',(-0.179147820429239,-3.48038656567466,
7.2420523320965));
#8493=CARTESIAN_POINT('Ctrl Pts',(-0.165439388560693,-3.4940951352783,7.1213117854776));
#8494=CARTESIAN_POINT('Ctrl Pts',(-0.0797949579373658,-3.50775053636266,
7.03576635961576));
#8495=CARTESIAN_POINT('Ctrl Pts',(0.0401637289317659,-3.52136611451607,
7.02224445826465));
#8496=CARTESIAN_POINT('Ctrl Pts',(0.142198917848681,-3.53496290502824,7.08647253741509));
#8497=CARTESIAN_POINT('Ctrl Pts',(0.168714822472972,-3.54401637293365,7.16206440300629));
#8498=CARTESIAN_POINT('Ctrl Pts',(0.16871996439457,-3.54855210247603,7.20017653463026));
#8499=CARTESIAN_POINT('Ctrl Pts',(0.199999521685004,-2.62021022067982,7.20354528529548));
#8500=CARTESIAN_POINT('Ctrl Pts',(0.19999343949118,-2.6255753643916,7.24862669087077));
#8501=CARTESIAN_POINT('Ctrl Pts',(0.168615691452697,-2.63634781999191,7.33868016798294));
#8502=CARTESIAN_POINT('Ctrl Pts',(0.0459616996448183,-2.65270477799173,
7.41618164971903));
#8503=CARTESIAN_POINT('Ctrl Pts',(-0.0998469869656992,-2.66924595959392,
7.39996507729611));
#8504=CARTESIAN_POINT('Ctrl Pts',(-0.204936181985623,-2.68597304189578,
7.29527847685269));
#8505=CARTESIAN_POINT('Ctrl Pts',(-0.221986969755699,-2.7028797483455,7.14628505326925));
#8506=CARTESIAN_POINT('Ctrl Pts',(-0.141631327334848,-2.71996166380803,
7.01788664502262));
#8507=CARTESIAN_POINT('Ctrl Pts',(0.00270481241442624,-2.73721192504324,
6.96708134679183));
#8508=CARTESIAN_POINT('Ctrl Pts',(0.143039113459417,-2.75397833948373,7.01603761180454));
#8509=CARTESIAN_POINT('Ctrl Pts',(0.223330027417085,-2.77023316539608,7.13370506584288));
#8510=CARTESIAN_POINT('Ctrl Pts',(0.223609433092684,-2.7859516486779,7.2713911725354));
#8511=CARTESIAN_POINT('Ctrl Pts',(0.152101468687107,-2.80045790761646,7.37648984952004));
#8512=CARTESIAN_POINT('Ctrl Pts',(0.0493840180807327,-2.81371750007274,
7.42583309513969));
#8513=CARTESIAN_POINT('Ctrl Pts',(-0.0535656424988984,-2.82570326133932,
7.42596307871198));
#8514=CARTESIAN_POINT('Ctrl Pts',(-0.146731811694293,-2.83773755003964,
7.38108373553243));
#8515=CARTESIAN_POINT('Ctrl Pts',(-0.211512387655128,-2.8498166397957,7.29998894076038));
#8516=CARTESIAN_POINT('Ctrl Pts',(-0.234672692510252,-2.86193666288461,
7.19851881716116));
#8517=CARTESIAN_POINT('Ctrl Pts',(-0.211502078818359,-2.87409363541626,
7.09651570260184));
#8518=CARTESIAN_POINT('Ctrl Pts',(-0.146175031667225,-2.88628349462379,
7.01496045942807));
#8519=CARTESIAN_POINT('Ctrl Pts',(-0.0201759406699065,-2.90257490033143,
6.95334279019282));
#8520=CARTESIAN_POINT('Ctrl Pts',(0.164048433167981,-2.92300029227989,6.99488705015939));
#8521=CARTESIAN_POINT('Ctrl Pts',(0.263212640482471,-2.94757377707087,7.20034626829039));
#8522=CARTESIAN_POINT('Ctrl Pts',(0.16413428164115,-2.9721746956776,7.40571604889496));
#8523=CARTESIAN_POINT('Ctrl Pts',(-0.0580809020736254,-2.99676718133414,
7.45651943873815));
#8524=CARTESIAN_POINT('Ctrl Pts',(-0.236127517621773,-3.02131545740765,
7.31427023254914));
#8525=CARTESIAN_POINT('Ctrl Pts',(-0.235623291843773,-3.04374517395574,
7.10674242176483));
#8526=CARTESIAN_POINT('Ctrl Pts',(-0.107269644782094,-3.06405280900675,
6.97972425972366));
#8527=CARTESIAN_POINT('Ctrl Pts',(0.0527757922260713,-3.08225163138773,
6.96159979137369));
#8528=CARTESIAN_POINT('Ctrl Pts',(0.188726377923501,-3.10035885514916,7.04734634676648));
#8529=CARTESIAN_POINT('Ctrl Pts',(0.232341637226282,-3.11536108595312,7.17289318656827));
#8530=CARTESIAN_POINT('Ctrl Pts',(0.215074929637344,-3.12730445561105,7.27290788199928));
#8531=CARTESIAN_POINT('Ctrl Pts',(0.166334604203376,-3.13920694864625,7.3615533699487));
#8532=CARTESIAN_POINT('Ctrl Pts',(0.0552567235661542,-3.1540048293497,7.43128948802867));
#8533=CARTESIAN_POINT('Ctrl Pts',(-0.100043793704833,-3.17162317434127,
7.4135433615447));
#8534=CARTESIAN_POINT('Ctrl Pts',(-0.209398878386583,-3.18909256344761,
7.30384381469642));
#8535=CARTESIAN_POINT('Ctrl Pts',(-0.226357160076232,-3.20640410002376,
7.15124619930781));
#8536=CARTESIAN_POINT('Ctrl Pts',(-0.145244888291477,-3.22354989628281,
7.02263774678675));
#8537=CARTESIAN_POINT('Ctrl Pts',(-0.00307739889558988,-3.24052311289208,
6.9731562179116));
#8538=CARTESIAN_POINT('Ctrl Pts',(0.137388780060693,-3.25731801286151,7.02262233145429));
#8539=CARTESIAN_POINT('Ctrl Pts',(0.215568012201749,-3.27392998789316,7.14745036721));
#8540=CARTESIAN_POINT('Ctrl Pts',(0.199056669422034,-3.29035561704227,7.29224338602279));
#8541=CARTESIAN_POINT('Ctrl Pts',(0.0972442378117872,-3.30659260084323,
7.39359267072072));
#8542=CARTESIAN_POINT('Ctrl Pts',(-0.0606078656788346,-3.32442299860284,
7.41159207397961));
#8543=CARTESIAN_POINT('Ctrl Pts',(-0.174349434794334,-3.34024917344643,
7.3202399790036));
#8544=CARTESIAN_POINT('Ctrl Pts',(-0.200242071600934,-3.35415023112003,
7.20325404432313));
#8545=CARTESIAN_POINT('Ctrl Pts',(-0.18063258547865,-3.36449358017806,7.11681410663695));
#8546=CARTESIAN_POINT('Ctrl Pts',(-0.125490051337178,-3.37475550369447,
7.04788845684967));
#8547=CARTESIAN_POINT('Ctrl Pts',(-0.0466957223057233,-3.38493729013136,
7.00998942647324));
#8548=CARTESIAN_POINT('Ctrl Pts',(0.0401186427931673,-3.39504044724382,
7.01009457046437));
#8549=CARTESIAN_POINT('Ctrl Pts',(0.117713403951327,-3.40506669595631,7.04749596858793));
#8550=CARTESIAN_POINT('Ctrl Pts',(0.170930387597076,-3.41501799177983,7.11440539415709));
#8551=CARTESIAN_POINT('Ctrl Pts',(0.18979238088286,-3.42489648282701,7.1971524208448));
#8552=CARTESIAN_POINT('Ctrl Pts',(0.17093827709221,-3.43470453492267,7.2792766512254));
#8553=CARTESIAN_POINT('Ctrl Pts',(0.123087817102158,-3.44363304446436,7.33923456804198));
#8554=CARTESIAN_POINT('Ctrl Pts',(0.0630389653927126,-3.45170235370222,
7.37229315652779));
#8555=CARTESIAN_POINT('Ctrl Pts',(-0.0177036729288226,-3.46133839204526,
7.38615351281265));
#8556=CARTESIAN_POINT('Ctrl Pts',(-0.11772305137169,-3.47329787855213,7.35109019812551));
#8557=CARTESIAN_POINT('Ctrl Pts',(-0.184714685581635,-3.48752403008714,
7.24410703240861));
#8558=CARTESIAN_POINT('Ctrl Pts',(-0.17053859750796,-3.50163575663314,7.11977423357787));
#8559=CARTESIAN_POINT('Ctrl Pts',(-0.082587996452088,-3.51564730527911,
7.03201669890537));
#8560=CARTESIAN_POINT('Ctrl Pts',(0.0401074098738201,-3.52956782204744,
7.0182572369454));
#8561=CARTESIAN_POINT('Ctrl Pts',(0.144033604536224,-3.54341977713357,7.08377705773452));
#8562=CARTESIAN_POINT('Ctrl Pts',(0.170884312908661,-3.55260377562906,7.16051919899628));
#8563=CARTESIAN_POINT('Ctrl Pts',(0.170889524395514,-3.55720086923049,7.1991469511116));
#8564=CARTESIAN_POINT('',(0.199999521685004,-2.62021022067982,7.20354528529548));
#8565=CARTESIAN_POINT('Origin',(0.2,-2.65,7.2));
#8566=CARTESIAN_POINT('',(0.170889524395514,-3.55720086923049,7.1991469511116));
#8567=CARTESIAN_POINT('Ctrl Pts',(0.199999521685004,-2.62021022067982,7.20354528529548));
#8568=CARTESIAN_POINT('Ctrl Pts',(0.19999343949118,-2.6255753643916,7.24862669087077));
#8569=CARTESIAN_POINT('Ctrl Pts',(0.168615691452697,-2.63634781999191,7.33868016798294));
#8570=CARTESIAN_POINT('Ctrl Pts',(0.0459616996448183,-2.65270477799173,
7.41618164971903));
#8571=CARTESIAN_POINT('Ctrl Pts',(-0.0998469869656992,-2.66924595959392,
7.39996507729611));
#8572=CARTESIAN_POINT('Ctrl Pts',(-0.204936181985623,-2.68597304189578,
7.29527847685269));
#8573=CARTESIAN_POINT('Ctrl Pts',(-0.221986969755699,-2.7028797483455,7.14628505326925));
#8574=CARTESIAN_POINT('Ctrl Pts',(-0.141631327334848,-2.71996166380803,
7.01788664502262));
#8575=CARTESIAN_POINT('Ctrl Pts',(0.00270481241442624,-2.73721192504324,
6.96708134679183));
#8576=CARTESIAN_POINT('Ctrl Pts',(0.143039113459417,-2.75397833948373,7.01603761180454));
#8577=CARTESIAN_POINT('Ctrl Pts',(0.223330027417085,-2.77023316539608,7.13370506584288));
#8578=CARTESIAN_POINT('Ctrl Pts',(0.223609433092684,-2.7859516486779,7.2713911725354));
#8579=CARTESIAN_POINT('Ctrl Pts',(0.152101468687107,-2.80045790761646,7.37648984952004));
#8580=CARTESIAN_POINT('Ctrl Pts',(0.0493840180807327,-2.81371750007274,
7.42583309513969));
#8581=CARTESIAN_POINT('Ctrl Pts',(-0.0535656424988984,-2.82570326133932,
7.42596307871198));
#8582=CARTESIAN_POINT('Ctrl Pts',(-0.146731811694293,-2.83773755003964,
7.38108373553243));
#8583=CARTESIAN_POINT('Ctrl Pts',(-0.211512387655128,-2.8498166397957,7.29998894076038));
#8584=CARTESIAN_POINT('Ctrl Pts',(-0.234672692510252,-2.86193666288461,
7.19851881716116));
#8585=CARTESIAN_POINT('Ctrl Pts',(-0.211502078818359,-2.87409363541626,
7.09651570260184));
#8586=CARTESIAN_POINT('Ctrl Pts',(-0.146175031667225,-2.88628349462379,
7.01496045942807));
#8587=CARTESIAN_POINT('Ctrl Pts',(-0.0201759406699065,-2.90257490033143,
6.95334279019282));
#8588=CARTESIAN_POINT('Ctrl Pts',(0.164048433167981,-2.92300029227989,6.99488705015939));
#8589=CARTESIAN_POINT('Ctrl Pts',(0.263212640482471,-2.94757377707087,7.20034626829039));
#8590=CARTESIAN_POINT('Ctrl Pts',(0.16413428164115,-2.9721746956776,7.40571604889496));
#8591=CARTESIAN_POINT('Ctrl Pts',(-0.0580809020736254,-2.99676718133414,
7.45651943873815));
#8592=CARTESIAN_POINT('Ctrl Pts',(-0.236127517621773,-3.02131545740765,
7.31427023254914));
#8593=CARTESIAN_POINT('Ctrl Pts',(-0.235623291843773,-3.04374517395574,
7.10674242176483));
#8594=CARTESIAN_POINT('Ctrl Pts',(-0.107269644782094,-3.06405280900675,
6.97972425972366));
#8595=CARTESIAN_POINT('Ctrl Pts',(0.0527757922260713,-3.08225163138773,
6.96159979137369));
#8596=CARTESIAN_POINT('Ctrl Pts',(0.188726377923501,-3.10035885514916,7.04734634676648));
#8597=CARTESIAN_POINT('Ctrl Pts',(0.232341637226282,-3.11536108595312,7.17289318656827));
#8598=CARTESIAN_POINT('Ctrl Pts',(0.215074929637344,-3.12730445561105,7.27290788199928));
#8599=CARTESIAN_POINT('Ctrl Pts',(0.166334604203376,-3.13920694864625,7.3615533699487));
#8600=CARTESIAN_POINT('Ctrl Pts',(0.0552567235661542,-3.1540048293497,7.43128948802867));
#8601=CARTESIAN_POINT('Ctrl Pts',(-0.100043793704833,-3.17162317434127,
7.4135433615447));
#8602=CARTESIAN_POINT('Ctrl Pts',(-0.209398878386583,-3.18909256344761,
7.30384381469642));
#8603=CARTESIAN_POINT('Ctrl Pts',(-0.226357160076232,-3.20640410002376,
7.15124619930781));
#8604=CARTESIAN_POINT('Ctrl Pts',(-0.145244888291477,-3.22354989628281,
7.02263774678675));
#8605=CARTESIAN_POINT('Ctrl Pts',(-0.00307739889558988,-3.24052311289208,
6.9731562179116));
#8606=CARTESIAN_POINT('Ctrl Pts',(0.137388780060693,-3.25731801286151,7.02262233145429));
#8607=CARTESIAN_POINT('Ctrl Pts',(0.215568012201749,-3.27392998789316,7.14745036721));
#8608=CARTESIAN_POINT('Ctrl Pts',(0.199056669422034,-3.29035561704227,7.29224338602279));
#8609=CARTESIAN_POINT('Ctrl Pts',(0.0972442378117872,-3.30659260084323,
7.39359267072072));
#8610=CARTESIAN_POINT('Ctrl Pts',(-0.0606078656788346,-3.32442299860284,
7.41159207397961));
#8611=CARTESIAN_POINT('Ctrl Pts',(-0.174349434794334,-3.34024917344643,
7.3202399790036));
#8612=CARTESIAN_POINT('Ctrl Pts',(-0.200242071600934,-3.35415023112003,
7.20325404432313));
#8613=CARTESIAN_POINT('Ctrl Pts',(-0.18063258547865,-3.36449358017806,7.11681410663695));
#8614=CARTESIAN_POINT('Ctrl Pts',(-0.125490051337178,-3.37475550369447,
7.04788845684967));
#8615=CARTESIAN_POINT('Ctrl Pts',(-0.0466957223057233,-3.38493729013136,
7.00998942647324));
#8616=CARTESIAN_POINT('Ctrl Pts',(0.0401186427931673,-3.39504044724382,
7.01009457046437));
#8617=CARTESIAN_POINT('Ctrl Pts',(0.117713403951327,-3.40506669595631,7.04749596858793));
#8618=CARTESIAN_POINT('Ctrl Pts',(0.170930387597076,-3.41501799177983,7.11440539415709));
#8619=CARTESIAN_POINT('Ctrl Pts',(0.18979238088286,-3.42489648282701,7.1971524208448));
#8620=CARTESIAN_POINT('Ctrl Pts',(0.17093827709221,-3.43470453492267,7.2792766512254));
#8621=CARTESIAN_POINT('Ctrl Pts',(0.123087817102158,-3.44363304446436,7.33923456804198));
#8622=CARTESIAN_POINT('Ctrl Pts',(0.0630389653927126,-3.45170235370222,
7.37229315652779));
#8623=CARTESIAN_POINT('Ctrl Pts',(-0.0177036729288226,-3.46133839204526,
7.38615351281265));
#8624=CARTESIAN_POINT('Ctrl Pts',(-0.11772305137169,-3.47329787855213,7.35109019812551));
#8625=CARTESIAN_POINT('Ctrl Pts',(-0.184714685581635,-3.48752403008714,
7.24410703240861));
#8626=CARTESIAN_POINT('Ctrl Pts',(-0.17053859750796,-3.50163575663314,7.11977423357787));
#8627=CARTESIAN_POINT('Ctrl Pts',(-0.082587996452088,-3.51564730527911,
7.03201669890537));
#8628=CARTESIAN_POINT('Ctrl Pts',(0.0401074098738201,-3.52956782204744,
7.0182572369454));
#8629=CARTESIAN_POINT('Ctrl Pts',(0.144033604536224,-3.54341977713357,7.08377705773452));
#8630=CARTESIAN_POINT('Ctrl Pts',(0.170884312908661,-3.55260377562906,7.16051919899628));
#8631=CARTESIAN_POINT('Ctrl Pts',(0.170889524395514,-3.55720086923049,7.1991469511116));
#8632=CARTESIAN_POINT('Origin',(0.2,-3.55,7.2));
#8633=CARTESIAN_POINT('Origin',(0.2,-3.55,7.2));
#8634=CARTESIAN_POINT('Origin',(0.2,-2.65,7.2));
#8635=CARTESIAN_POINT('',(0.,0.,0.));
#8636=CARTESIAN_POINT('Origin',(-0.6,11.,0.));
#8637=CARTESIAN_POINT('',(-0.6,11.,0.));
#8638=CARTESIAN_POINT('',(-1.3,11.,0.));
#8639=CARTESIAN_POINT('',(-0.6,11.,0.));
#8640=CARTESIAN_POINT('',(-1.3,11.,6.));
#8641=CARTESIAN_POINT('',(-1.3,11.,0.));
#8642=CARTESIAN_POINT('',(-0.6,11.,6.));
#8643=CARTESIAN_POINT('',(-0.6,11.,6.));
#8644=CARTESIAN_POINT('',(-0.6,11.,0.));
#8645=CARTESIAN_POINT('Origin',(-0.6,9.5,0.));
#8646=CARTESIAN_POINT('',(-0.6,9.5,0.));
#8647=CARTESIAN_POINT('',(-0.6,9.5,0.));
#8648=CARTESIAN_POINT('',(-0.6,9.5,6.));
#8649=CARTESIAN_POINT('',(-0.6,9.5,6.));
#8650=CARTESIAN_POINT('',(-0.6,9.5,0.));
#8651=CARTESIAN_POINT('Origin',(-1.3,9.5,0.));
#8652=CARTESIAN_POINT('',(-1.3,9.5,0.));
#8653=CARTESIAN_POINT('',(-1.3,9.5,0.));
#8654=CARTESIAN_POINT('',(-1.3,9.5,6.));
#8655=CARTESIAN_POINT('',(-1.3,9.5,6.));
#8656=CARTESIAN_POINT('',(-1.3,9.5,0.));
#8657=CARTESIAN_POINT('Origin',(-1.3,11.,0.));
#8658=CARTESIAN_POINT('',(-1.3,11.,0.));
#8659=CARTESIAN_POINT('',(-1.3,11.,6.));
#8660=CARTESIAN_POINT('Origin',(-0.95,10.25,6.));
#8661=CARTESIAN_POINT('Origin',(-0.95,10.25,0.));
#8662=CARTESIAN_POINT('',(0.,0.,0.));
#8663=CARTESIAN_POINT('Origin',(-0.3,11.,0.));
#8664=CARTESIAN_POINT('',(-0.3,11.,0.));
#8665=CARTESIAN_POINT('',(-0.6,11.,0.));
#8666=CARTESIAN_POINT('',(-0.3,11.,0.));
#8667=CARTESIAN_POINT('',(-0.6,11.,6.));
#8668=CARTESIAN_POINT('',(-0.6,11.,0.));
#8669=CARTESIAN_POINT('',(-0.3,11.,6.));
#8670=CARTESIAN_POINT('',(-0.3,11.,6.));
#8671=CARTESIAN_POINT('',(-0.3,11.,0.));
#8672=CARTESIAN_POINT('Origin',(-0.3,9.5,0.));
#8673=CARTESIAN_POINT('',(-0.3,9.5,0.));
#8674=CARTESIAN_POINT('',(-0.3,9.5,0.));
#8675=CARTESIAN_POINT('',(-0.3,9.5,6.));
#8676=CARTESIAN_POINT('',(-0.3,9.5,6.));
#8677=CARTESIAN_POINT('',(-0.3,9.5,0.));
#8678=CARTESIAN_POINT('Origin',(-0.6,9.5,0.));
#8679=CARTESIAN_POINT('',(-0.6,9.5,0.));
#8680=CARTESIAN_POINT('',(-0.6,9.5,0.));
#8681=CARTESIAN_POINT('',(-0.6,9.5,6.));
#8682=CARTESIAN_POINT('',(-0.6,9.5,6.));
#8683=CARTESIAN_POINT('',(-0.6,9.5,0.));
#8684=CARTESIAN_POINT('Origin',(-0.6,11.,0.));
#8685=CARTESIAN_POINT('',(-0.6,11.,0.));
#8686=CARTESIAN_POINT('',(-0.6,11.,6.));
#8687=CARTESIAN_POINT('Origin',(-0.45,10.25,6.));
#8688=CARTESIAN_POINT('Origin',(-0.45,10.25,0.));
#8689=CARTESIAN_POINT('',(0.,0.,0.));
#8690=CARTESIAN_POINT('Origin',(0.,0.,0.));
#8691=CARTESIAN_POINT('',(-0.32,0.16,3.91886975727153E-17));
#8692=CARTESIAN_POINT('Origin',(0.,0.16,0.));
#8693=CARTESIAN_POINT('',(-0.32,0.,3.91886975727153E-17));
#8694=CARTESIAN_POINT('',(-0.32,0.,3.91886975727153E-17));
#8695=CARTESIAN_POINT('Origin',(0.,0.,0.));
#8696=CARTESIAN_POINT('Origin',(0.,0.,0.));
#8697=CARTESIAN_POINT('',(-0.6,0.16,7.34788079488412E-17));
#8698=CARTESIAN_POINT('Origin',(0.,0.16,0.));
#8699=CARTESIAN_POINT('',(-0.6,0.,7.34788079488412E-17));
#8700=CARTESIAN_POINT('',(-0.6,0.,7.34788079488412E-17));
#8701=CARTESIAN_POINT('Origin',(0.,0.,0.));
#8702=CARTESIAN_POINT('Origin',(0.,0.16,0.));
#8703=CARTESIAN_POINT('Origin',(0.,0.,0.));
#8704=CARTESIAN_POINT('',(0.,0.,0.));
#8705=CARTESIAN_POINT('Origin',(0.144337567297406,-0.6,-0.25));
#8706=CARTESIAN_POINT('',(0.288675134594813,-0.6,0.));
#8707=CARTESIAN_POINT('',(0.144337567297406,-0.6,-0.25));
#8708=CARTESIAN_POINT('',(0.288675134594813,-0.6,0.));
#8709=CARTESIAN_POINT('',(0.144337567297406,-0.96,-0.25));
#8710=CARTESIAN_POINT('',(0.144337567297406,-0.6,-0.25));
#8711=CARTESIAN_POINT('',(0.288675134594813,-0.96,0.));
#8712=CARTESIAN_POINT('',(0.288675134594813,-0.96,0.));
#8713=CARTESIAN_POINT('',(0.288675134594813,-0.6,0.));
#8714=CARTESIAN_POINT('Origin',(-0.144337567297406,-0.6,-0.25));
#8715=CARTESIAN_POINT('',(-0.144337567297406,-0.6,-0.25));
#8716=CARTESIAN_POINT('',(0.144337567297406,-0.6,-0.25));
#8717=CARTESIAN_POINT('',(-0.144337567297406,-0.96,-0.25));
#8718=CARTESIAN_POINT('',(-0.144337567297406,-0.6,-0.25));
#8719=CARTESIAN_POINT('',(0.144337567297406,-0.96,-0.25));
#8720=CARTESIAN_POINT('Origin',(-0.288675134594813,-0.6,-8.32667268468867E-17));
#8721=CARTESIAN_POINT('',(-0.288675134594813,-0.6,-3.53525079574969E-17));
#8722=CARTESIAN_POINT('',(-0.144337567297406,-0.6,-0.25));
#8723=CARTESIAN_POINT('',(-0.288675134594813,-0.96,-5.55111512312578E-17));
#8724=CARTESIAN_POINT('',(-0.288675134594813,-0.6,-3.53525079574969E-17));
#8725=CARTESIAN_POINT('',(-0.144337567297406,-0.96,-0.25));
#8726=CARTESIAN_POINT('Origin',(-0.144337567297407,-0.6,0.25));
#8727=CARTESIAN_POINT('',(-0.144337567297407,-0.6,0.25));
#8728=CARTESIAN_POINT('',(-0.288675134594813,-0.6,-3.53525079574969E-17));
#8729=CARTESIAN_POINT('',(-0.144337567297407,-0.96,0.25));
#8730=CARTESIAN_POINT('',(-0.144337567297407,-0.6,0.25));
#8731=CARTESIAN_POINT('',(-0.288675134594813,-0.96,-3.53525079574969E-17));
#8732=CARTESIAN_POINT('Origin',(0.144337567297406,-0.6,0.25));
#8733=CARTESIAN_POINT('',(0.144337567297406,-0.6,0.25));
#8734=CARTESIAN_POINT('',(-0.144337567297407,-0.6,0.25));
#8735=CARTESIAN_POINT('',(0.144337567297406,-0.96,0.25));
#8736=CARTESIAN_POINT('',(0.144337567297406,-0.6,0.25));
#8737=CARTESIAN_POINT('',(-0.144337567297407,-0.96,0.25));
#8738=CARTESIAN_POINT('Origin',(0.288675134594813,-0.6,0.));
#8739=CARTESIAN_POINT('',(0.144337567297406,-0.6,0.25));
#8740=CARTESIAN_POINT('',(0.144337567297406,-0.96,0.25));
#8741=CARTESIAN_POINT('Origin',(0.,-0.6,0.));
#8742=CARTESIAN_POINT('Origin',(0.,-0.96,0.));
#8743=CARTESIAN_POINT('Origin',(0.,-1.8,0.));
#8744=CARTESIAN_POINT('',(-0.2942,-1.8,3.60291088309151E-17));
#8745=CARTESIAN_POINT('Origin',(0.,-1.8,0.));
#8746=CARTESIAN_POINT('Origin',(0.45,0.6,0.));
#8747=CARTESIAN_POINT('',(-0.45,0.6,-5.51091059616309E-17));
#8748=CARTESIAN_POINT('Origin',(0.,0.6,0.));
#8749=CARTESIAN_POINT('Origin',(0.,0.575,0.));
#8750=CARTESIAN_POINT('',(-0.5,0.55,-6.12323399573677E-17));
#8751=CARTESIAN_POINT('Origin',(0.,0.55,0.));
#8752=CARTESIAN_POINT('',(-0.475,0.575,-5.81707229594993E-17));
#8753=CARTESIAN_POINT('Origin',(0.,0.29,0.));
#8754=CARTESIAN_POINT('',(-0.5,0.0299999999999998,-6.12323399573677E-17));
#8755=CARTESIAN_POINT('Origin',(0.,0.0299999999999998,0.));
#8756=CARTESIAN_POINT('',(-0.5,0.29,-6.12323399573677E-17));
#8757=CARTESIAN_POINT('Origin',(0.,0.0150000000000001,0.));
#8758=CARTESIAN_POINT('',(-0.47,7.11236625150491E-17,-5.75583995599256E-17));
#8759=CARTESIAN_POINT('Origin',(0.,0.,0.));
#8760=CARTESIAN_POINT('',(-0.485,0.0150000000000001,-5.93953697586466E-17));
#8761=CARTESIAN_POINT('Origin',(0.32,0.,0.));
#8762=CARTESIAN_POINT('',(-0.32,-6.93889390390723E-18,-3.91886975727153E-17));
#8763=CARTESIAN_POINT('Origin',(0.,0.,0.));
#8764=CARTESIAN_POINT('Origin',(0.,-0.02,0.));
#8765=CARTESIAN_POINT('',(-0.2942,-0.0515999999999999,3.60291088309151E-17));
#8766=CARTESIAN_POINT('Origin',(0.,-0.0515999999999999,0.));
#8767=CARTESIAN_POINT('',(-0.31,-0.02,-3.7964050773568E-17));
#8768=CARTESIAN_POINT('Origin',(0.,-1.24,0.));
#8769=CARTESIAN_POINT('',(-0.2942,-1.24,-3.60291088309151E-17));
#8770=CARTESIAN_POINT('',(0.,0.,0.));
#8771=CARTESIAN_POINT('',(0.,0.,0.));
#8772=CARTESIAN_POINT('Origin',(0.,0.,0.));
#8773=CARTESIAN_POINT('',(-0.976185,-0.246528389340863,-1.19548183562566E-16));
#8774=CARTESIAN_POINT('',(-1.19548183562566E-16,-0.246528389340863,0.976185));
#8775=CARTESIAN_POINT('Origin',(0.,-0.246528389340863,0.));
#8776=CARTESIAN_POINT('Origin',(0.,-0.246528389340863,0.));
#8777=CARTESIAN_POINT('',(-1.19548183562566E-16,0.246528389340863,0.976185));
#8778=CARTESIAN_POINT('Origin',(-1.22464679914735E-16,0.,1.));
#8779=CARTESIAN_POINT('',(-0.976185,0.246528389340863,1.19548183562566E-16));
#8780=CARTESIAN_POINT('Origin',(0.,0.246528389340863,0.));
#8781=CARTESIAN_POINT('Origin',(0.,0.246528389340863,0.));
#8782=CARTESIAN_POINT('Origin',(0.,0.,0.));
#8783=CARTESIAN_POINT('',(-0.976185,0.45,-1.19548183562566E-16));
#8784=CARTESIAN_POINT('',(-0.976185,0.,-1.19548183562566E-16));
#8785=CARTESIAN_POINT('Origin',(0.,0.45,0.));
#8786=CARTESIAN_POINT('Origin',(0.,0.,0.));
#8787=CARTESIAN_POINT('',(-0.5,-0.39,-6.12323399573677E-17));
#8788=CARTESIAN_POINT('Origin',(0.,-0.39,0.));
#8789=CARTESIAN_POINT('',(-0.5,0.39,-6.12323399573677E-17));
#8790=CARTESIAN_POINT('',(-0.5,0.,-6.12323399573677E-17));
#8791=CARTESIAN_POINT('Origin',(0.,0.39,0.));
#8792=CARTESIAN_POINT('Origin',(0.,0.42,0.));
#8793=CARTESIAN_POINT('',(-0.56,0.45,-6.85802207522518E-17));
#8794=CARTESIAN_POINT('',(-0.53,0.42,-6.49062803548097E-17));
#8795=CARTESIAN_POINT('Origin',(0.,0.45,0.));
#8796=CARTESIAN_POINT('Origin',(0.976185,0.45,0.));
#8797=CARTESIAN_POINT('Origin',(0.,0.,0.));
#8798=CARTESIAN_POINT('',(-0.976185,-0.45,-1.19548183562566E-16));
#8799=CARTESIAN_POINT('Origin',(0.,-0.45,0.));
#8800=CARTESIAN_POINT('',(-0.976185,0.,-1.19548183562566E-16));
#8801=CARTESIAN_POINT('Origin',(0.56,-0.45,0.));
#8802=CARTESIAN_POINT('',(-0.56,-0.45,-6.85802207522518E-17));
#8803=CARTESIAN_POINT('Origin',(0.,-0.45,0.));
#8804=CARTESIAN_POINT('Origin',(0.,-0.42,0.));
#8805=CARTESIAN_POINT('',(-0.53,-0.42,-6.49062803548097E-17));
#8806=CARTESIAN_POINT('',(0.,0.,0.));
#8807=CARTESIAN_POINT('Origin',(0.,0.,0.));
#8808=CARTESIAN_POINT('',(-1.023815,0.246528389340863,-1.25381176266905E-16));
#8809=CARTESIAN_POINT('',(-1.25381176266905E-16,0.246528389340863,1.023815));
#8810=CARTESIAN_POINT('Origin',(0.,0.246528389340863,0.));
#8811=CARTESIAN_POINT('Origin',(0.,0.246528389340863,0.));
#8812=CARTESIAN_POINT('',(-1.25381176266905E-16,-0.246528389340863,1.023815));
#8813=CARTESIAN_POINT('Origin',(-1.22464679914735E-16,0.,1.));
#8814=CARTESIAN_POINT('',(-1.023815,-0.246528389340863,1.25381176266905E-16));
#8815=CARTESIAN_POINT('Origin',(0.,-0.246528389340863,0.));
#8816=CARTESIAN_POINT('Origin',(0.,-0.246528389340863,0.));
#8817=CARTESIAN_POINT('Origin',(0.,0.,0.));
#8818=CARTESIAN_POINT('',(-1.023815,-0.45,-1.25381176266905E-16));
#8819=CARTESIAN_POINT('Origin',(0.,-0.45,0.));
#8820=CARTESIAN_POINT('',(-1.023815,0.,-1.25381176266905E-16));
#8821=CARTESIAN_POINT('Origin',(1.44,0.45,0.));
#8822=CARTESIAN_POINT('',(-1.44,0.45,-1.76349139077219E-16));
#8823=CARTESIAN_POINT('Origin',(0.,0.45,0.));
#8824=CARTESIAN_POINT('',(-1.023815,0.45,-1.25381176266905E-16));
#8825=CARTESIAN_POINT('Origin',(0.,0.45,0.));
#8826=CARTESIAN_POINT('Origin',(0.,0.42,0.));
#8827=CARTESIAN_POINT('',(-1.5,0.39,-1.83697019872103E-16));
#8828=CARTESIAN_POINT('Origin',(0.,0.39,0.));
#8829=CARTESIAN_POINT('',(-1.47,0.42,-1.80023079474661E-16));
#8830=CARTESIAN_POINT('Origin',(0.,0.,0.));
#8831=CARTESIAN_POINT('',(-1.5,-0.39,-1.83697019872103E-16));
#8832=CARTESIAN_POINT('Origin',(0.,-0.39,0.));
#8833=CARTESIAN_POINT('',(-1.5,0.,-1.83697019872103E-16));
#8834=CARTESIAN_POINT('Origin',(0.,-0.42,0.));
#8835=CARTESIAN_POINT('',(-1.44,-0.45,-1.76349139077219E-16));
#8836=CARTESIAN_POINT('Origin',(0.,-0.45,0.));
#8837=CARTESIAN_POINT('',(-1.47,-0.42,-1.80023079474661E-16));
#8838=CARTESIAN_POINT('Origin',(1.023815,-0.45,0.));
#8839=CARTESIAN_POINT('Origin',(0.,0.,0.));
#8840=CARTESIAN_POINT('',(-1.023815,0.,-1.25381176266905E-16));
#8841=CARTESIAN_POINT('',(0.,0.,0.));
#8842=CARTESIAN_POINT('Origin',(1.,0.,0.));
#8843=CARTESIAN_POINT('',(1.,-1.78583896120461E-33,0.23815));
#8844=CARTESIAN_POINT('',(1.,-1.78583896120461E-33,-0.23815));
#8845=CARTESIAN_POINT('Origin',(1.,0.,0.));
#8846=CARTESIAN_POINT('Origin',(0.707106781186548,0.,-0.707106781186547));
#8847=CARTESIAN_POINT('',(0.875504261126124,-1.78583896120461E-33,-0.538709301246971));
#8848=CARTESIAN_POINT('',(0.538709301246971,-1.78583896120461E-33,-0.875504261126124));
#8849=CARTESIAN_POINT('Origin',(0.707106781186548,0.,-0.707106781186547));
#8850=CARTESIAN_POINT('Origin',(6.12323399573677E-17,0.,-1.));
#8851=CARTESIAN_POINT('',(0.23815,-1.78583896120461E-33,-1.));
#8852=CARTESIAN_POINT('',(-0.23815,-1.78583896120461E-33,-1.));
#8853=CARTESIAN_POINT('Origin',(6.12323399573677E-17,0.,-1.));
#8854=CARTESIAN_POINT('Origin',(-0.707106781186547,0.,-0.707106781186548));
#8855=CARTESIAN_POINT('',(-0.538709301246971,-1.78583896120461E-33,-0.875504261126124));
#8856=CARTESIAN_POINT('',(-0.875504261126124,-1.78583896120461E-33,-0.538709301246971));
#8857=CARTESIAN_POINT('Origin',(-0.707106781186547,0.,-0.707106781186548));
#8858=CARTESIAN_POINT('Origin',(-1.,0.,-1.22464679914735E-16));
#8859=CARTESIAN_POINT('',(-1.,-1.78583896120461E-33,-0.23815));
#8860=CARTESIAN_POINT('',(-1.,-1.78583896120461E-33,0.23815));
#8861=CARTESIAN_POINT('Origin',(-1.,0.,-1.22464679914735E-16));
#8862=CARTESIAN_POINT('Origin',(-0.707106781186548,0.,0.707106781186547));
#8863=CARTESIAN_POINT('',(-0.875504261126124,-7.94881478324376E-33,0.538709301246971));
#8864=CARTESIAN_POINT('',(-0.538709301246971,4.37713686083455E-33,0.875504261126124));
#8865=CARTESIAN_POINT('Origin',(-0.707106781186548,0.,0.707106781186547));
#8866=CARTESIAN_POINT('Origin',(-1.83697019872103E-16,0.,1.));
#8867=CARTESIAN_POINT('',(-0.23815,-1.78583896120461E-33,1.));
#8868=CARTESIAN_POINT('',(0.23815,-1.78583896120461E-33,1.));
#8869=CARTESIAN_POINT('Origin',(-1.83697019872103E-16,0.,1.));
#8870=CARTESIAN_POINT('Origin',(0.707106781186547,0.,0.707106781186548));
#8871=CARTESIAN_POINT('',(0.538709301246971,-4.86732687222419E-33,0.875504261126124));
#8872=CARTESIAN_POINT('',(0.875504261126124,1.29564894981497E-33,0.538709301246971));
#8873=CARTESIAN_POINT('Origin',(0.707106781186547,0.,0.707106781186548));
#8874=CARTESIAN_POINT('',(0.,0.,0.));
#8875=CARTESIAN_POINT('Origin',(0.707106781186547,0.,0.707106781186548));
#8876=CARTESIAN_POINT('',(0.504455939115715,-0.04763,0.841298510752802));
#8877=CARTESIAN_POINT('',(0.841298510752802,-0.04763,0.504455939115715));
#8878=CARTESIAN_POINT('Ctrl Pts',(0.504455939115715,-0.04763,0.841298510752802));
#8879=CARTESIAN_POINT('Ctrl Pts',(0.508899795931835,-0.0740444353928835,
0.838633903678357));
#8880=CARTESIAN_POINT('Ctrl Pts',(0.517157748491652,-0.0999305678883309,
0.833661031856294));
#8881=CARTESIAN_POINT('Ctrl Pts',(0.537715343527944,-0.142345102874864,
0.820511285096538));
#8882=CARTESIAN_POINT('Ctrl Pts',(0.548874290046456,-0.159766064500479,
0.813159949759));
#8883=CARTESIAN_POINT('Ctrl Pts',(0.573915184558107,-0.190326085855194,
0.795684265985089));
#8884=CARTESIAN_POINT('Ctrl Pts',(0.587792702767295,-0.203463743702801,
0.78555112003688));
#8885=CARTESIAN_POINT('Ctrl Pts',(0.615966552324775,-0.224161999508995,
0.763642258217233));
#8886=CARTESIAN_POINT('Ctrl Pts',(0.631684198665438,-0.232861760990032,
0.750785745543687));
#8887=CARTESIAN_POINT('Ctrl Pts',(0.663382628119203,-0.244251601209411,
0.722929908501543));
#8888=CARTESIAN_POINT('Ctrl Pts',(0.679352081686668,-0.246942143572133,
0.707917883896095));
#8889=CARTESIAN_POINT('Ctrl Pts',(0.707917883896095,-0.246942143572133,
0.679352081686668));
#8890=CARTESIAN_POINT('Ctrl Pts',(0.722929908501543,-0.244251601209411,
0.663382628119203));
#8891=CARTESIAN_POINT('Ctrl Pts',(0.750785745543687,-0.232861760990032,
0.631684198665439));
#8892=CARTESIAN_POINT('Ctrl Pts',(0.763642258217232,-0.224161999508995,
0.615966552324775));
#8893=CARTESIAN_POINT('Ctrl Pts',(0.78555112003688,-0.203463743702801,0.587792702767295));
#8894=CARTESIAN_POINT('Ctrl Pts',(0.795684265985088,-0.190326085855194,
0.573915184558108));
#8895=CARTESIAN_POINT('Ctrl Pts',(0.813159949759,-0.15976606450048,0.548874290046456));
#8896=CARTESIAN_POINT('Ctrl Pts',(0.820511285096538,-0.142345102874864,
0.537715343527944));
#8897=CARTESIAN_POINT('Ctrl Pts',(0.833661031856294,-0.099930567888331,
0.517157748491653));
#8898=CARTESIAN_POINT('Ctrl Pts',(0.838633903678357,-0.0740444353928835,
0.508899795931835));
#8899=CARTESIAN_POINT('Ctrl Pts',(0.841298510752801,-0.0476299999999999,
0.504455939115715));
#8900=CARTESIAN_POINT('',(0.528110872004958,-0.04763,0.871530771444223));
#8901=CARTESIAN_POINT('Origin',(0.707106781186547,-0.04763,0.707106781186548));
#8902=CARTESIAN_POINT('',(0.871530771444223,-0.04763,0.528110872004959));
#8903=CARTESIAN_POINT('Ctrl Pts',(0.871530771444223,-0.0476300000000001,
0.528110872004958));
#8904=CARTESIAN_POINT('Ctrl Pts',(0.87014664509073,-0.0609922781173483,
0.530395067942936));
#8905=CARTESIAN_POINT('Ctrl Pts',(0.868149331745851,-0.0742967091364493,
0.533674141594226));
#8906=CARTESIAN_POINT('Ctrl Pts',(0.85981294420286,-0.115492077056649,0.54708917182331));
#8907=CARTESIAN_POINT('Ctrl Pts',(0.850993704737257,-0.141695629206859,
0.560922177770136));
#8908=CARTESIAN_POINT('Ctrl Pts',(0.830754510485543,-0.181890537957859,
0.590422647829571));
#8909=CARTESIAN_POINT('Ctrl Pts',(0.816896541396381,-0.201072148666545,
0.609616703125488));
#8910=CARTESIAN_POINT('Ctrl Pts',(0.792310597819928,-0.223955109275652,
0.641117951819998));
#8911=CARTESIAN_POINT('Ctrl Pts',(0.779109323683612,-0.232742381310829,
0.657208095763053));
#8912=CARTESIAN_POINT('Ctrl Pts',(0.750552691816206,-0.244234834628584,
0.68964083160521));
#8913=CARTESIAN_POINT('Ctrl Pts',(0.735185187071673,-0.246942143572133,
0.705971972091755));
#8914=CARTESIAN_POINT('Ctrl Pts',(0.705971972091754,-0.246942143572133,
0.735185187071673));
#8915=CARTESIAN_POINT('Ctrl Pts',(0.689640831605209,-0.244234834628584,
0.750552691816206));
#8916=CARTESIAN_POINT('Ctrl Pts',(0.657208095763052,-0.232742381310829,
0.779109323683612));
#8917=CARTESIAN_POINT('Ctrl Pts',(0.641117951819998,-0.223955109275652,
0.792310597819928));
#8918=CARTESIAN_POINT('Ctrl Pts',(0.609616703125487,-0.201072148666545,
0.816896541396382));
#8919=CARTESIAN_POINT('Ctrl Pts',(0.590422647829571,-0.181890537957858,
0.830754510485544));
#8920=CARTESIAN_POINT('Ctrl Pts',(0.560922177770135,-0.141695629206858,
0.850993704737257));
#8921=CARTESIAN_POINT('Ctrl Pts',(0.547089171823309,-0.115492077056649,
0.859812944202861));
#8922=CARTESIAN_POINT('Ctrl Pts',(0.533674141594226,-0.0742967091364491,
0.868149331745852));
#8923=CARTESIAN_POINT('Ctrl Pts',(0.530395067942936,-0.0609922781173483,
0.870146645090731));
#8924=CARTESIAN_POINT('Ctrl Pts',(0.528110872004958,-0.0476300000000001,
0.871530771444223));
#8925=CARTESIAN_POINT('Origin',(0.707106781186547,-0.04763,0.707106781186548));
#8926=CARTESIAN_POINT('Origin',(0.,-0.166705,0.));
#8927=CARTESIAN_POINT('',(0.242834539687906,-0.04763,0.989696097314));
#8928=CARTESIAN_POINT('Origin',(0.,-0.04763,0.));
#8929=CARTESIAN_POINT('',(-0.242834539687907,-0.04763,0.989696097314));
#8930=CARTESIAN_POINT('Ctrl Pts',(0.242834539687906,-0.04763,0.989696097314));
#8931=CARTESIAN_POINT('Ctrl Pts',(0.24024064412003,-0.0609922781173483,
0.990332542620729));
#8932=CARTESIAN_POINT('Ctrl Pts',(0.236509675094874,-0.0742967091364492,
0.991238884025248));
#8933=CARTESIAN_POINT('Ctrl Pts',(0.221129100087819,-0.115492077056649,
0.994830026707808));
#8934=CARTESIAN_POINT('Ctrl Pts',(0.205111543747588,-0.141695629206859,
0.998375294985966));
#8935=CARTESIAN_POINT('Ctrl Pts',(0.169940289819232,-0.181890537957859,
1.00492400591205));
#8936=CARTESIAN_POINT('Ctrl Pts',(0.1465689792446,-0.201072148666545,1.00869718865384));
#8937=CARTESIAN_POINT('Ctrl Pts',(0.106909345252087,-0.223955109275652,
1.01358704779679));
#8938=CARTESIAN_POINT('Ctrl Pts',(0.0861971848975941,-0.232742381310829,
1.0156297872271));
#8939=CARTESIAN_POINT('Ctrl Pts',(0.0430711894098822,-0.244234834628584,
1.01837060663223));
#8940=CARTESIAN_POINT('Ctrl Pts',(0.0206568624125605,-0.246942143572133,
1.019052));
#8941=CARTESIAN_POINT('Ctrl Pts',(-0.0206568624125608,-0.246942143572133,
1.019052));
#8942=CARTESIAN_POINT('Ctrl Pts',(-0.0430711894098825,-0.244234834628584,
1.01837060663223));
#8943=CARTESIAN_POINT('Ctrl Pts',(-0.0861971848975943,-0.232742381310829,
1.0156297872271));
#8944=CARTESIAN_POINT('Ctrl Pts',(-0.106909345252088,-0.223955109275652,
1.01358704779679));
#8945=CARTESIAN_POINT('Ctrl Pts',(-0.1465689792446,-0.201072148666545,1.00869718865384));
#8946=CARTESIAN_POINT('Ctrl Pts',(-0.169940289819232,-0.181890537957859,
1.00492400591205));
#8947=CARTESIAN_POINT('Ctrl Pts',(-0.205111543747588,-0.141695629206859,
0.998375294985966));
#8948=CARTESIAN_POINT('Ctrl Pts',(-0.221129100087819,-0.115492077056649,
0.994830026707808));
#8949=CARTESIAN_POINT('Ctrl Pts',(-0.236509675094875,-0.0742967091364493,
0.991238884025248));
#8950=CARTESIAN_POINT('Ctrl Pts',(-0.24024064412003,-0.0609922781173483,
0.990332542620729));
#8951=CARTESIAN_POINT('Ctrl Pts',(-0.242834539687907,-0.04763,0.989696097314));
#8952=CARTESIAN_POINT('',(-0.528110872004959,-0.04763,0.871530771444223));
#8953=CARTESIAN_POINT('Origin',(0.,-0.04763,0.));
#8954=CARTESIAN_POINT('',(-0.871530771444223,-0.04763,0.528110872004958));
#8955=CARTESIAN_POINT('Ctrl Pts',(-0.528110872004958,-0.0476300000000001,
0.871530771444223));
#8956=CARTESIAN_POINT('Ctrl Pts',(-0.530395067942936,-0.0609922781173484,
0.87014664509073));
#8957=CARTESIAN_POINT('Ctrl Pts',(-0.533674141594226,-0.0742967091364493,
0.868149331745851));
#8958=CARTESIAN_POINT('Ctrl Pts',(-0.54708917182331,-0.115492077056649,
0.85981294420286));
#8959=CARTESIAN_POINT('Ctrl Pts',(-0.560922177770136,-0.141695629206859,
0.850993704737257));
#8960=CARTESIAN_POINT('Ctrl Pts',(-0.590422647829571,-0.181890537957859,
0.830754510485543));
#8961=CARTESIAN_POINT('Ctrl Pts',(-0.609616703125488,-0.201072148666545,
0.816896541396381));
#8962=CARTESIAN_POINT('Ctrl Pts',(-0.641117951819998,-0.223955109275652,
0.792310597819928));
#8963=CARTESIAN_POINT('Ctrl Pts',(-0.657208095763053,-0.232742381310829,
0.779109323683611));
#8964=CARTESIAN_POINT('Ctrl Pts',(-0.68964083160521,-0.244234834628584,
0.750552691816205));
#8965=CARTESIAN_POINT('Ctrl Pts',(-0.705971972091755,-0.246942143572133,
0.735185187071673));
#8966=CARTESIAN_POINT('Ctrl Pts',(-0.735185187071673,-0.246942143572133,
0.705971972091754));
#8967=CARTESIAN_POINT('Ctrl Pts',(-0.750552691816206,-0.244234834628584,
0.689640831605209));
#8968=CARTESIAN_POINT('Ctrl Pts',(-0.779109323683612,-0.232742381310829,
0.657208095763052));
#8969=CARTESIAN_POINT('Ctrl Pts',(-0.792310597819928,-0.223955109275652,
0.641117951819998));
#8970=CARTESIAN_POINT('Ctrl Pts',(-0.816896541396382,-0.201072148666545,
0.609616703125487));
#8971=CARTESIAN_POINT('Ctrl Pts',(-0.830754510485544,-0.181890537957858,
0.590422647829571));
#8972=CARTESIAN_POINT('Ctrl Pts',(-0.850993704737257,-0.141695629206858,
0.560922177770135));
#8973=CARTESIAN_POINT('Ctrl Pts',(-0.859812944202861,-0.115492077056649,
0.547089171823309));
#8974=CARTESIAN_POINT('Ctrl Pts',(-0.868149331745852,-0.0742967091364491,
0.533674141594226));
#8975=CARTESIAN_POINT('Ctrl Pts',(-0.870146645090731,-0.0609922781173483,
0.530395067942936));
#8976=CARTESIAN_POINT('Ctrl Pts',(-0.871530771444223,-0.04763,0.528110872004958));
#8977=CARTESIAN_POINT('',(-0.989696097314,-0.04763,0.242834539687906));
#8978=CARTESIAN_POINT('Origin',(0.,-0.04763,0.));
#8979=CARTESIAN_POINT('',(-1.019052,-0.246942143572133,1.248489836334E-16));
#8980=CARTESIAN_POINT('Ctrl Pts',(-0.989696097314,-0.04763,0.242834539687906));
#8981=CARTESIAN_POINT('Ctrl Pts',(-0.990332542620729,-0.0609922781173483,
0.24024064412003));
#8982=CARTESIAN_POINT('Ctrl Pts',(-0.991238884025248,-0.0742967091364492,
0.236509675094874));
#8983=CARTESIAN_POINT('Ctrl Pts',(-0.994830026707808,-0.115492077056649,
0.221129100087819));
#8984=CARTESIAN_POINT('Ctrl Pts',(-0.998375294985966,-0.141695629206859,
0.205111543747588));
#8985=CARTESIAN_POINT('Ctrl Pts',(-1.00492400591205,-0.181890537957859,
0.169940289819232));
#8986=CARTESIAN_POINT('Ctrl Pts',(-1.00869718865384,-0.201072148666545,
0.1465689792446));
#8987=CARTESIAN_POINT('Ctrl Pts',(-1.01358704779679,-0.223955109275652,
0.106909345252088));
#8988=CARTESIAN_POINT('Ctrl Pts',(-1.0156297872271,-0.232742381310829,0.0861971848975944));
#8989=CARTESIAN_POINT('Ctrl Pts',(-1.01837060663223,-0.244234834628584,
0.0430711894098825));
#8990=CARTESIAN_POINT('Ctrl Pts',(-1.019052,-0.246942143572133,0.0206568624125608));
#8991=CARTESIAN_POINT('Ctrl Pts',(-1.019052,-0.246942143572133,1.2490009027033E-16));
#8992=CARTESIAN_POINT('',(-1.019052,-0.28578,1.24797876996471E-16));
#8993=CARTESIAN_POINT('',(-1.019052,-0.166705,1.24797876996471E-16));
#8994=CARTESIAN_POINT('Origin',(0.,-0.28578,0.));
#8995=CARTESIAN_POINT('',(-0.989696097314,-0.04763,-0.242834539687906));
#8996=CARTESIAN_POINT('Ctrl Pts',(-1.019052,-0.246942143572133,1.2490009027033E-16));
#8997=CARTESIAN_POINT('Ctrl Pts',(-1.019052,-0.246942143572133,-0.0206568624125605));
#8998=CARTESIAN_POINT('Ctrl Pts',(-1.01837060663223,-0.244234834628584,
-0.0430711894098822));
#8999=CARTESIAN_POINT('Ctrl Pts',(-1.0156297872271,-0.232742381310829,-0.0861971848975941));
#9000=CARTESIAN_POINT('Ctrl Pts',(-1.01358704779679,-0.223955109275652,
-0.106909345252087));
#9001=CARTESIAN_POINT('Ctrl Pts',(-1.00869718865384,-0.201072148666546,
-0.1465689792446));
#9002=CARTESIAN_POINT('Ctrl Pts',(-1.00492400591205,-0.181890537957859,
-0.169940289819232));
#9003=CARTESIAN_POINT('Ctrl Pts',(-0.998375294985966,-0.141695629206859,
-0.205111543747588));
#9004=CARTESIAN_POINT('Ctrl Pts',(-0.994830026707808,-0.11549207705665,
-0.221129100087819));
#9005=CARTESIAN_POINT('Ctrl Pts',(-0.991238884025248,-0.0742967091364495,
-0.236509675094874));
#9006=CARTESIAN_POINT('Ctrl Pts',(-0.990332542620729,-0.0609922781173484,
-0.24024064412003));
#9007=CARTESIAN_POINT('Ctrl Pts',(-0.989696097314,-0.0476300000000001,-0.242834539687907));
#9008=CARTESIAN_POINT('',(-0.871530771444223,-0.04763,-0.528110872004958));
#9009=CARTESIAN_POINT('Origin',(0.,-0.04763,0.));
#9010=CARTESIAN_POINT('',(-0.528110872004958,-0.04763,-0.871530771444223));
#9011=CARTESIAN_POINT('Ctrl Pts',(-0.871530771444223,-0.0476300000000001,
-0.528110872004958));
#9012=CARTESIAN_POINT('Ctrl Pts',(-0.87014664509073,-0.0609922781173484,
-0.530395067942936));
#9013=CARTESIAN_POINT('Ctrl Pts',(-0.868149331745851,-0.0742967091364494,
-0.533674141594226));
#9014=CARTESIAN_POINT('Ctrl Pts',(-0.85981294420286,-0.115492077056649,
-0.54708917182331));
#9015=CARTESIAN_POINT('Ctrl Pts',(-0.850993704737257,-0.141695629206859,
-0.560922177770136));
#9016=CARTESIAN_POINT('Ctrl Pts',(-0.830754510485543,-0.181890537957859,
-0.590422647829571));
#9017=CARTESIAN_POINT('Ctrl Pts',(-0.816896541396381,-0.201072148666546,
-0.609616703125488));
#9018=CARTESIAN_POINT('Ctrl Pts',(-0.792310597819928,-0.223955109275652,
-0.641117951819999));
#9019=CARTESIAN_POINT('Ctrl Pts',(-0.779109323683611,-0.232742381310829,
-0.657208095763053));
#9020=CARTESIAN_POINT('Ctrl Pts',(-0.750552691816205,-0.244234834628584,
-0.68964083160521));
#9021=CARTESIAN_POINT('Ctrl Pts',(-0.735185187071673,-0.246942143572133,
-0.705971972091755));
#9022=CARTESIAN_POINT('Ctrl Pts',(-0.705971972091754,-0.246942143572133,
-0.735185187071673));
#9023=CARTESIAN_POINT('Ctrl Pts',(-0.68964083160521,-0.244234834628584,
-0.750552691816206));
#9024=CARTESIAN_POINT('Ctrl Pts',(-0.657208095763052,-0.232742381310829,
-0.779109323683612));
#9025=CARTESIAN_POINT('Ctrl Pts',(-0.641117951819998,-0.223955109275652,
-0.792310597819928));
#9026=CARTESIAN_POINT('Ctrl Pts',(-0.609616703125488,-0.201072148666545,
-0.816896541396381));
#9027=CARTESIAN_POINT('Ctrl Pts',(-0.590422647829571,-0.181890537957859,
-0.830754510485543));
#9028=CARTESIAN_POINT('Ctrl Pts',(-0.560922177770136,-0.141695629206859,
-0.850993704737257));
#9029=CARTESIAN_POINT('Ctrl Pts',(-0.54708917182331,-0.115492077056649,
-0.85981294420286));
#9030=CARTESIAN_POINT('Ctrl Pts',(-0.533674141594226,-0.0742967091364494,
-0.868149331745852));
#9031=CARTESIAN_POINT('Ctrl Pts',(-0.530395067942936,-0.0609922781173484,
-0.870146645090731));
#9032=CARTESIAN_POINT('Ctrl Pts',(-0.528110872004958,-0.0476300000000001,
-0.871530771444223));
#9033=CARTESIAN_POINT('',(-0.242834539687906,-0.04763,-0.989696097314));
#9034=CARTESIAN_POINT('Origin',(0.,-0.04763,0.));
#9035=CARTESIAN_POINT('',(0.242834539687906,-0.04763,-0.989696097314));
#9036=CARTESIAN_POINT('Ctrl Pts',(-0.242834539687907,-0.04763,-0.989696097314));
#9037=CARTESIAN_POINT('Ctrl Pts',(-0.24024064412003,-0.0609922781173483,
-0.990332542620729));
#9038=CARTESIAN_POINT('Ctrl Pts',(-0.236509675094874,-0.0742967091364493,
-0.991238884025248));
#9039=CARTESIAN_POINT('Ctrl Pts',(-0.221129100087819,-0.115492077056649,
-0.994830026707808));
#9040=CARTESIAN_POINT('Ctrl Pts',(-0.205111543747588,-0.141695629206859,
-0.998375294985966));
#9041=CARTESIAN_POINT('Ctrl Pts',(-0.169940289819232,-0.181890537957859,
-1.00492400591205));
#9042=CARTESIAN_POINT('Ctrl Pts',(-0.1465689792446,-0.201072148666545,-1.00869718865384));
#9043=CARTESIAN_POINT('Ctrl Pts',(-0.106909345252087,-0.223955109275652,
-1.01358704779679));
#9044=CARTESIAN_POINT('Ctrl Pts',(-0.0861971848975942,-0.232742381310829,
-1.0156297872271));
#9045=CARTESIAN_POINT('Ctrl Pts',(-0.0430711894098823,-0.244234834628584,
-1.01837060663223));
#9046=CARTESIAN_POINT('Ctrl Pts',(-0.0206568624125606,-0.246942143572133,
-1.019052));
#9047=CARTESIAN_POINT('Ctrl Pts',(0.0206568624125607,-0.246942143572133,
-1.019052));
#9048=CARTESIAN_POINT('Ctrl Pts',(0.0430711894098824,-0.244234834628584,
-1.01837060663223));
#9049=CARTESIAN_POINT('Ctrl Pts',(0.0861971848975943,-0.232742381310829,
-1.0156297872271));
#9050=CARTESIAN_POINT('Ctrl Pts',(0.106909345252088,-0.223955109275652,
-1.01358704779679));
#9051=CARTESIAN_POINT('Ctrl Pts',(0.1465689792446,-0.201072148666545,-1.00869718865384));
#9052=CARTESIAN_POINT('Ctrl Pts',(0.169940289819232,-0.181890537957859,
-1.00492400591205));
#9053=CARTESIAN_POINT('Ctrl Pts',(0.205111543747588,-0.141695629206859,
-0.998375294985966));
#9054=CARTESIAN_POINT('Ctrl Pts',(0.221129100087819,-0.115492077056649,
-0.994830026707808));
#9055=CARTESIAN_POINT('Ctrl Pts',(0.236509675094874,-0.0742967091364493,
-0.991238884025248));
#9056=CARTESIAN_POINT('Ctrl Pts',(0.24024064412003,-0.0609922781173484,
-0.990332542620729));
#9057=CARTESIAN_POINT('Ctrl Pts',(0.242834539687907,-0.04763,-0.989696097314));
#9058=CARTESIAN_POINT('',(0.528110872004958,-0.04763,-0.871530771444223));
#9059=CARTESIAN_POINT('Origin',(0.,-0.04763,0.));
#9060=CARTESIAN_POINT('',(0.871530771444223,-0.04763,-0.528110872004958));
#9061=CARTESIAN_POINT('Ctrl Pts',(0.528110872004958,-0.0476300000000001,
-0.871530771444223));
#9062=CARTESIAN_POINT('Ctrl Pts',(0.530395067942936,-0.0609922781173484,
-0.870146645090731));
#9063=CARTESIAN_POINT('Ctrl Pts',(0.533674141594226,-0.0742967091364493,
-0.868149331745851));
#9064=CARTESIAN_POINT('Ctrl Pts',(0.54708917182331,-0.115492077056649,-0.85981294420286));
#9065=CARTESIAN_POINT('Ctrl Pts',(0.560922177770136,-0.141695629206859,
-0.850993704737257));
#9066=CARTESIAN_POINT('Ctrl Pts',(0.590422647829571,-0.181890537957859,
-0.830754510485543));
#9067=CARTESIAN_POINT('Ctrl Pts',(0.609616703125488,-0.201072148666545,
-0.816896541396381));
#9068=CARTESIAN_POINT('Ctrl Pts',(0.641117951819998,-0.223955109275652,
-0.792310597819928));
#9069=CARTESIAN_POINT('Ctrl Pts',(0.657208095763053,-0.232742381310829,
-0.779109323683612));
#9070=CARTESIAN_POINT('Ctrl Pts',(0.68964083160521,-0.244234834628584,-0.750552691816206));
#9071=CARTESIAN_POINT('Ctrl Pts',(0.705971972091755,-0.246942143572133,
-0.735185187071673));
#9072=CARTESIAN_POINT('Ctrl Pts',(0.735185187071673,-0.246942143572133,
-0.705971972091754));
#9073=CARTESIAN_POINT('Ctrl Pts',(0.750552691816206,-0.244234834628584,
-0.68964083160521));
#9074=CARTESIAN_POINT('Ctrl Pts',(0.779109323683612,-0.232742381310829,
-0.657208095763053));
#9075=CARTESIAN_POINT('Ctrl Pts',(0.792310597819928,-0.223955109275652,
-0.641117951819998));
#9076=CARTESIAN_POINT('Ctrl Pts',(0.816896541396381,-0.201072148666545,
-0.609616703125488));
#9077=CARTESIAN_POINT('Ctrl Pts',(0.830754510485543,-0.181890537957859,
-0.590422647829571));
#9078=CARTESIAN_POINT('Ctrl Pts',(0.850993704737257,-0.141695629206859,
-0.560922177770136));
#9079=CARTESIAN_POINT('Ctrl Pts',(0.85981294420286,-0.115492077056649,-0.54708917182331));
#9080=CARTESIAN_POINT('Ctrl Pts',(0.868149331745851,-0.0742967091364493,
-0.533674141594226));
#9081=CARTESIAN_POINT('Ctrl Pts',(0.870146645090731,-0.0609922781173484,
-0.530395067942936));
#9082=CARTESIAN_POINT('Ctrl Pts',(0.871530771444223,-0.0476300000000001,
-0.528110872004958));
#9083=CARTESIAN_POINT('',(0.989696097314,-0.04763,-0.242834539687906));
#9084=CARTESIAN_POINT('Origin',(0.,-0.04763,0.));
#9085=CARTESIAN_POINT('',(0.989696097314,-0.04763,0.242834539687906));
#9086=CARTESIAN_POINT('Ctrl Pts',(0.989696097314,-0.04763,-0.242834539687907));
#9087=CARTESIAN_POINT('Ctrl Pts',(0.990332542620729,-0.0609922781173483,
-0.24024064412003));
#9088=CARTESIAN_POINT('Ctrl Pts',(0.991238884025248,-0.0742967091364493,
-0.236509675094874));
#9089=CARTESIAN_POINT('Ctrl Pts',(0.994830026707808,-0.115492077056649,
-0.221129100087819));
#9090=CARTESIAN_POINT('Ctrl Pts',(0.998375294985966,-0.141695629206859,
-0.205111543747588));
#9091=CARTESIAN_POINT('Ctrl Pts',(1.00492400591205,-0.181890537957859,-0.169940289819232));
#9092=CARTESIAN_POINT('Ctrl Pts',(1.00869718865384,-0.201072148666545,-0.1465689792446));
#9093=CARTESIAN_POINT('Ctrl Pts',(1.01358704779679,-0.223955109275652,-0.106909345252087));
#9094=CARTESIAN_POINT('Ctrl Pts',(1.0156297872271,-0.232742381310829,-0.0861971848975942));
#9095=CARTESIAN_POINT('Ctrl Pts',(1.01837060663223,-0.244234834628584,-0.0430711894098823));
#9096=CARTESIAN_POINT('Ctrl Pts',(1.019052,-0.246942143572133,-0.0206568624125607));
#9097=CARTESIAN_POINT('Ctrl Pts',(1.019052,-0.246942143572133,0.0206568624125607));
#9098=CARTESIAN_POINT('Ctrl Pts',(1.01837060663223,-0.244234834628584,0.0430711894098823));
#9099=CARTESIAN_POINT('Ctrl Pts',(1.0156297872271,-0.232742381310829,0.0861971848975942));
#9100=CARTESIAN_POINT('Ctrl Pts',(1.01358704779679,-0.223955109275652,0.106909345252087));
#9101=CARTESIAN_POINT('Ctrl Pts',(1.00869718865384,-0.201072148666545,0.1465689792446));
#9102=CARTESIAN_POINT('Ctrl Pts',(1.00492400591205,-0.181890537957859,0.169940289819232));
#9103=CARTESIAN_POINT('Ctrl Pts',(0.998375294985966,-0.141695629206859,
0.205111543747588));
#9104=CARTESIAN_POINT('Ctrl Pts',(0.994830026707808,-0.115492077056649,
0.221129100087819));
#9105=CARTESIAN_POINT('Ctrl Pts',(0.991238884025248,-0.0742967091364492,
0.236509675094874));
#9106=CARTESIAN_POINT('Ctrl Pts',(0.990332542620729,-0.0609922781173483,
0.24024064412003));
#9107=CARTESIAN_POINT('Ctrl Pts',(0.989696097314,-0.04763,0.242834539687907));
#9108=CARTESIAN_POINT('Origin',(0.,-0.04763,0.));
#9109=CARTESIAN_POINT('Origin',(0.,-0.04763,0.));
#9110=CARTESIAN_POINT('',(0.238183666596899,-0.04763,0.951592097314));
#9111=CARTESIAN_POINT('Origin',(0.,-0.04763,0.));
#9112=CARTESIAN_POINT('Origin',(-1.94289029309402E-16,-0.04763,1.));
#9113=CARTESIAN_POINT('Origin',(-1.94289029309402E-16,0.,1.));
#9114=CARTESIAN_POINT('',(-0.2381836665969,-0.04763,0.951592097314));
#9115=CARTESIAN_POINT('Ctrl Pts',(-0.238183666596899,-0.0476299999999999,
0.951592097314));
#9116=CARTESIAN_POINT('Ctrl Pts',(-0.233157223576062,-0.0740444353928835,
0.952850216871763));
#9117=CARTESIAN_POINT('Ctrl Pts',(-0.223801617934946,-0.0999305678883309,
0.955173119738174));
#9118=CARTESIAN_POINT('Ctrl Pts',(-0.199966927975188,-0.142345102874864,
0.960411259488514));
#9119=CARTESIAN_POINT('Ctrl Pts',(-0.1868781821531,-0.159766064500479,0.963103647174702));
#9120=CARTESIAN_POINT('Ctrl Pts',(-0.15681442133453,-0.190326085855194,
0.968453058988463));
#9121=CARTESIAN_POINT('Ctrl Pts',(-0.139836317888043,-0.203463743702801,
0.971100730005489));
#9122=CARTESIAN_POINT('Ctrl Pts',(-0.104422493053067,-0.224161999508995,
0.975530745318961));
#9123=CARTESIAN_POINT('Ctrl Pts',(-0.0842175114474176,-0.232861760990032,
0.977553872336861));
#9124=CARTESIAN_POINT('Ctrl Pts',(-0.0421062857595701,-0.244251601209411,
0.980270995488453));
#9125=CARTESIAN_POINT('Ctrl Pts',(-0.0201990724523197,-0.246942143572133,
0.980948));
#9126=CARTESIAN_POINT('Ctrl Pts',(0.020199072452319,-0.246942143572133,
0.980948));
#9127=CARTESIAN_POINT('Ctrl Pts',(0.0421062857595694,-0.244251601209411,
0.980270995488454));
#9128=CARTESIAN_POINT('Ctrl Pts',(0.0842175114474169,-0.232861760990032,
0.977553872336861));
#9129=CARTESIAN_POINT('Ctrl Pts',(0.104422493053067,-0.224161999508995,
0.975530745318961));
#9130=CARTESIAN_POINT('Ctrl Pts',(0.139836317888042,-0.203463743702801,
0.971100730005489));
#9131=CARTESIAN_POINT('Ctrl Pts',(0.15681442133453,-0.190326085855194,0.968453058988463));
#9132=CARTESIAN_POINT('Ctrl Pts',(0.1868781821531,-0.15976606450048,0.963103647174702));
#9133=CARTESIAN_POINT('Ctrl Pts',(0.199966927975188,-0.142345102874864,
0.960411259488514));
#9134=CARTESIAN_POINT('Ctrl Pts',(0.223801617934945,-0.0999305678883309,
0.955173119738174));
#9135=CARTESIAN_POINT('Ctrl Pts',(0.233157223576061,-0.0740444353928835,
0.952850216871763));
#9136=CARTESIAN_POINT('Ctrl Pts',(0.238183666596899,-0.0476299999999999,
0.951592097314));
#9137=CARTESIAN_POINT('Origin',(-1.94289029309402E-16,-0.04763,1.));
#9138=CARTESIAN_POINT('Origin',(0.,-0.04763,0.));
#9139=CARTESIAN_POINT('',(-0.504455939115715,-0.04763,0.841298510752802));
#9140=CARTESIAN_POINT('Origin',(0.,-0.04763,0.));
#9141=CARTESIAN_POINT('Origin',(-0.707106781186548,-0.04763,0.707106781186547));
#9142=CARTESIAN_POINT('Origin',(-0.707106781186548,0.,0.707106781186547));
#9143=CARTESIAN_POINT('',(-0.841298510752802,-0.04763,0.504455939115715));
#9144=CARTESIAN_POINT('Ctrl Pts',(-0.841298510752802,-0.04763,0.504455939115715));
#9145=CARTESIAN_POINT('Ctrl Pts',(-0.838633903678357,-0.0740444353928835,
0.508899795931835));
#9146=CARTESIAN_POINT('Ctrl Pts',(-0.833661031856294,-0.0999305678883309,
0.517157748491652));
#9147=CARTESIAN_POINT('Ctrl Pts',(-0.820511285096538,-0.142345102874864,
0.537715343527944));
#9148=CARTESIAN_POINT('Ctrl Pts',(-0.813159949759,-0.159766064500479,0.548874290046456));
#9149=CARTESIAN_POINT('Ctrl Pts',(-0.795684265985089,-0.190326085855194,
0.573915184558107));
#9150=CARTESIAN_POINT('Ctrl Pts',(-0.78555112003688,-0.203463743702801,
0.587792702767295));
#9151=CARTESIAN_POINT('Ctrl Pts',(-0.763642258217233,-0.224161999508995,
0.615966552324775));
#9152=CARTESIAN_POINT('Ctrl Pts',(-0.750785745543687,-0.232861760990032,
0.631684198665438));
#9153=CARTESIAN_POINT('Ctrl Pts',(-0.722929908501543,-0.244251601209411,
0.663382628119203));
#9154=CARTESIAN_POINT('Ctrl Pts',(-0.707917883896095,-0.246942143572133,
0.679352081686668));
#9155=CARTESIAN_POINT('Ctrl Pts',(-0.679352081686668,-0.246942143572133,
0.707917883896095));
#9156=CARTESIAN_POINT('Ctrl Pts',(-0.663382628119203,-0.244251601209411,
0.722929908501544));
#9157=CARTESIAN_POINT('Ctrl Pts',(-0.631684198665438,-0.232861760990031,
0.750785745543687));
#9158=CARTESIAN_POINT('Ctrl Pts',(-0.615966552324775,-0.224161999508995,
0.763642258217233));
#9159=CARTESIAN_POINT('Ctrl Pts',(-0.587792702767295,-0.203463743702801,
0.78555112003688));
#9160=CARTESIAN_POINT('Ctrl Pts',(-0.573915184558107,-0.190326085855194,
0.795684265985088));
#9161=CARTESIAN_POINT('Ctrl Pts',(-0.548874290046456,-0.159766064500479,
0.813159949759));
#9162=CARTESIAN_POINT('Ctrl Pts',(-0.537715343527944,-0.142345102874864,
0.820511285096538));
#9163=CARTESIAN_POINT('Ctrl Pts',(-0.517157748491652,-0.0999305678883309,
0.833661031856294));
#9164=CARTESIAN_POINT('Ctrl Pts',(-0.508899795931835,-0.0740444353928835,
0.838633903678357));
#9165=CARTESIAN_POINT('Ctrl Pts',(-0.504455939115716,-0.04763,0.841298510752801));
#9166=CARTESIAN_POINT('Origin',(-0.707106781186548,-0.04763,0.707106781186547));
#9167=CARTESIAN_POINT('Origin',(0.,-0.04763,0.));
#9168=CARTESIAN_POINT('',(-0.951592097314,-0.04763,0.238183666596899));
#9169=CARTESIAN_POINT('Origin',(0.,-0.04763,0.));
#9170=CARTESIAN_POINT('Origin',(-1.,-0.04763,-1.11022302462516E-16));
#9171=CARTESIAN_POINT('Origin',(-1.,0.,-1.11022302462516E-16));
#9172=CARTESIAN_POINT('',(-0.951592097314,-0.04763,-0.2381836665969));
#9173=CARTESIAN_POINT('',(-0.980948,-0.246942143572133,1.08514323328844E-18));
#9174=CARTESIAN_POINT('Ctrl Pts',(-0.951592097314,-0.04763,-0.238183666596899));
#9175=CARTESIAN_POINT('Ctrl Pts',(-0.952850216871763,-0.0740444353928835,
-0.233157223576062));
#9176=CARTESIAN_POINT('Ctrl Pts',(-0.955173119738174,-0.0999305678883309,
-0.223801617934946));
#9177=CARTESIAN_POINT('Ctrl Pts',(-0.960411259488514,-0.142345102874864,
-0.199966927975188));
#9178=CARTESIAN_POINT('Ctrl Pts',(-0.963103647174702,-0.159766064500479,
-0.1868781821531));
#9179=CARTESIAN_POINT('Ctrl Pts',(-0.968453058988463,-0.190326085855194,
-0.15681442133453));
#9180=CARTESIAN_POINT('Ctrl Pts',(-0.971100730005489,-0.203463743702801,
-0.139836317888043));
#9181=CARTESIAN_POINT('Ctrl Pts',(-0.975530745318961,-0.224161999508995,
-0.104422493053067));
#9182=CARTESIAN_POINT('Ctrl Pts',(-0.977553872336861,-0.232861760990032,
-0.0842175114474175));
#9183=CARTESIAN_POINT('Ctrl Pts',(-0.980270995488453,-0.244251601209411,
-0.0421062857595699));
#9184=CARTESIAN_POINT('Ctrl Pts',(-0.980948,-0.246942143572133,-0.0201990724523195));
#9185=CARTESIAN_POINT('Ctrl Pts',(-0.980948,-0.246942143572133,-1.17961196366423E-16));
#9186=CARTESIAN_POINT('Origin',(-1.,-0.04763,-1.11022302462516E-16));
#9187=CARTESIAN_POINT('Ctrl Pts',(-0.980948,-0.246942143572133,-1.17961196366423E-16));
#9188=CARTESIAN_POINT('Ctrl Pts',(-0.980948,-0.246942143572133,0.0201990724523192));
#9189=CARTESIAN_POINT('Ctrl Pts',(-0.980270995488453,-0.244251601209411,
0.0421062857595695));
#9190=CARTESIAN_POINT('Ctrl Pts',(-0.977553872336861,-0.232861760990032,
0.0842175114474169));
#9191=CARTESIAN_POINT('Ctrl Pts',(-0.975530745318961,-0.224161999508995,
0.104422493053066));
#9192=CARTESIAN_POINT('Ctrl Pts',(-0.971100730005489,-0.203463743702801,
0.139836317888042));
#9193=CARTESIAN_POINT('Ctrl Pts',(-0.968453058988463,-0.190326085855194,
0.15681442133453));
#9194=CARTESIAN_POINT('Ctrl Pts',(-0.963103647174702,-0.15976606450048,
0.1868781821531));
#9195=CARTESIAN_POINT('Ctrl Pts',(-0.960411259488514,-0.142345102874864,
0.199966927975188));
#9196=CARTESIAN_POINT('Ctrl Pts',(-0.955173119738174,-0.099930567888331,
0.223801617934945));
#9197=CARTESIAN_POINT('Ctrl Pts',(-0.952850216871763,-0.0740444353928835,
0.233157223576061));
#9198=CARTESIAN_POINT('Ctrl Pts',(-0.951592097314,-0.04763,0.238183666596899));
#9199=CARTESIAN_POINT('Origin',(0.,-0.04763,0.));
#9200=CARTESIAN_POINT('',(-0.841298510752802,-0.04763,-0.504455939115715));
#9201=CARTESIAN_POINT('Origin',(0.,-0.04763,0.));
#9202=CARTESIAN_POINT('Origin',(-0.707106781186547,-0.04763,-0.707106781186548));
#9203=CARTESIAN_POINT('Origin',(-0.707106781186547,0.,-0.707106781186548));
#9204=CARTESIAN_POINT('',(-0.504455939115715,-0.04763,-0.841298510752802));
#9205=CARTESIAN_POINT('Ctrl Pts',(-0.504455939115715,-0.04763,-0.841298510752802));
#9206=CARTESIAN_POINT('Ctrl Pts',(-0.508899795931835,-0.0740444353928835,
-0.838633903678357));
#9207=CARTESIAN_POINT('Ctrl Pts',(-0.517157748491652,-0.0999305678883309,
-0.833661031856294));
#9208=CARTESIAN_POINT('Ctrl Pts',(-0.537715343527944,-0.142345102874864,
-0.820511285096538));
#9209=CARTESIAN_POINT('Ctrl Pts',(-0.548874290046456,-0.159766064500479,
-0.813159949759));
#9210=CARTESIAN_POINT('Ctrl Pts',(-0.573915184558107,-0.190326085855194,
-0.795684265985089));
#9211=CARTESIAN_POINT('Ctrl Pts',(-0.587792702767295,-0.203463743702801,
-0.78555112003688));
#9212=CARTESIAN_POINT('Ctrl Pts',(-0.615966552324775,-0.224161999508995,
-0.763642258217233));
#9213=CARTESIAN_POINT('Ctrl Pts',(-0.631684198665438,-0.232861760990032,
-0.750785745543687));
#9214=CARTESIAN_POINT('Ctrl Pts',(-0.663382628119203,-0.244251601209411,
-0.722929908501543));
#9215=CARTESIAN_POINT('Ctrl Pts',(-0.679352081686668,-0.246942143572133,
-0.707917883896095));
#9216=CARTESIAN_POINT('Ctrl Pts',(-0.707917883896095,-0.246942143572133,
-0.679352081686668));
#9217=CARTESIAN_POINT('Ctrl Pts',(-0.722929908501543,-0.244251601209411,
-0.663382628119203));
#9218=CARTESIAN_POINT('Ctrl Pts',(-0.750785745543687,-0.232861760990032,
-0.631684198665439));
#9219=CARTESIAN_POINT('Ctrl Pts',(-0.763642258217232,-0.224161999508995,
-0.615966552324775));
#9220=CARTESIAN_POINT('Ctrl Pts',(-0.78555112003688,-0.203463743702801,
-0.587792702767295));
#9221=CARTESIAN_POINT('Ctrl Pts',(-0.795684265985088,-0.190326085855194,
-0.573915184558107));
#9222=CARTESIAN_POINT('Ctrl Pts',(-0.813159949759,-0.15976606450048,-0.548874290046456));
#9223=CARTESIAN_POINT('Ctrl Pts',(-0.820511285096538,-0.142345102874864,
-0.537715343527944));
#9224=CARTESIAN_POINT('Ctrl Pts',(-0.833661031856294,-0.0999305678883311,
-0.517157748491652));
#9225=CARTESIAN_POINT('Ctrl Pts',(-0.838633903678357,-0.0740444353928836,
-0.508899795931835));
#9226=CARTESIAN_POINT('Ctrl Pts',(-0.841298510752801,-0.04763,-0.504455939115715));
#9227=CARTESIAN_POINT('Origin',(-0.707106781186547,-0.04763,-0.707106781186548));
#9228=CARTESIAN_POINT('Origin',(0.,-0.04763,0.));
#9229=CARTESIAN_POINT('',(-0.238183666596899,-0.04763,-0.951592097314));
#9230=CARTESIAN_POINT('Origin',(0.,-0.04763,0.));
#9231=CARTESIAN_POINT('Origin',(5.55111512312578E-17,-0.04763,-1.));
#9232=CARTESIAN_POINT('Origin',(5.55111512312578E-17,0.,-1.));
#9233=CARTESIAN_POINT('',(0.238183666596899,-0.04763,-0.951592097314));
#9234=CARTESIAN_POINT('Ctrl Pts',(0.238183666596899,-0.04763,-0.951592097314));
#9235=CARTESIAN_POINT('Ctrl Pts',(0.233157223576062,-0.0740444353928835,
-0.952850216871763));
#9236=CARTESIAN_POINT('Ctrl Pts',(0.223801617934946,-0.099930567888331,
-0.955173119738174));
#9237=CARTESIAN_POINT('Ctrl Pts',(0.199966927975188,-0.142345102874864,
-0.960411259488514));
#9238=CARTESIAN_POINT('Ctrl Pts',(0.1868781821531,-0.15976606450048,-0.963103647174702));
#9239=CARTESIAN_POINT('Ctrl Pts',(0.15681442133453,-0.190326085855194,-0.968453058988463));
#9240=CARTESIAN_POINT('Ctrl Pts',(0.139836317888042,-0.203463743702801,
-0.971100730005489));
#9241=CARTESIAN_POINT('Ctrl Pts',(0.104422493053067,-0.224161999508995,
-0.975530745318961));
#9242=CARTESIAN_POINT('Ctrl Pts',(0.0842175114474173,-0.232861760990032,
-0.977553872336861));
#9243=CARTESIAN_POINT('Ctrl Pts',(0.0421062857595698,-0.244251601209411,
-0.980270995488453));
#9244=CARTESIAN_POINT('Ctrl Pts',(0.0201990724523194,-0.246942143572133,
-0.980948));
#9245=CARTESIAN_POINT('Ctrl Pts',(-0.0201990724523193,-0.246942143572133,
-0.980948));
#9246=CARTESIAN_POINT('Ctrl Pts',(-0.0421062857595697,-0.244251601209411,
-0.980270995488453));
#9247=CARTESIAN_POINT('Ctrl Pts',(-0.0842175114474171,-0.232861760990032,
-0.977553872336861));
#9248=CARTESIAN_POINT('Ctrl Pts',(-0.104422493053067,-0.224161999508995,
-0.975530745318961));
#9249=CARTESIAN_POINT('Ctrl Pts',(-0.139836317888042,-0.203463743702801,
-0.971100730005489));
#9250=CARTESIAN_POINT('Ctrl Pts',(-0.15681442133453,-0.190326085855194,
-0.968453058988463));
#9251=CARTESIAN_POINT('Ctrl Pts',(-0.1868781821531,-0.15976606450048,-0.963103647174702));
#9252=CARTESIAN_POINT('Ctrl Pts',(-0.199966927975188,-0.142345102874864,
-0.960411259488514));
#9253=CARTESIAN_POINT('Ctrl Pts',(-0.223801617934945,-0.099930567888331,
-0.955173119738174));
#9254=CARTESIAN_POINT('Ctrl Pts',(-0.233157223576062,-0.0740444353928835,
-0.952850216871763));
#9255=CARTESIAN_POINT('Ctrl Pts',(-0.238183666596899,-0.0476299999999999,
-0.951592097314));
#9256=CARTESIAN_POINT('Origin',(5.55111512312578E-17,-0.04763,-1.));
#9257=CARTESIAN_POINT('Origin',(0.,-0.04763,0.));
#9258=CARTESIAN_POINT('',(0.504455939115715,-0.04763,-0.841298510752802));
#9259=CARTESIAN_POINT('Origin',(0.,-0.04763,0.));
#9260=CARTESIAN_POINT('Origin',(0.707106781186548,-0.04763,-0.707106781186547));
#9261=CARTESIAN_POINT('Origin',(0.707106781186548,0.,-0.707106781186547));
#9262=CARTESIAN_POINT('',(0.841298510752802,-0.04763,-0.504455939115715));
#9263=CARTESIAN_POINT('Ctrl Pts',(0.841298510752802,-0.04763,-0.504455939115715));
#9264=CARTESIAN_POINT('Ctrl Pts',(0.838633903678357,-0.0740444353928835,
-0.508899795931835));
#9265=CARTESIAN_POINT('Ctrl Pts',(0.833661031856294,-0.0999305678883309,
-0.517157748491652));
#9266=CARTESIAN_POINT('Ctrl Pts',(0.820511285096538,-0.142345102874864,
-0.537715343527944));
#9267=CARTESIAN_POINT('Ctrl Pts',(0.813159949759,-0.159766064500479,-0.548874290046456));
#9268=CARTESIAN_POINT('Ctrl Pts',(0.795684265985088,-0.190326085855194,
-0.573915184558107));
#9269=CARTESIAN_POINT('Ctrl Pts',(0.78555112003688,-0.203463743702801,-0.587792702767295));
#9270=CARTESIAN_POINT('Ctrl Pts',(0.763642258217233,-0.224161999508995,
-0.615966552324775));
#9271=CARTESIAN_POINT('Ctrl Pts',(0.750785745543687,-0.232861760990032,
-0.631684198665438));
#9272=CARTESIAN_POINT('Ctrl Pts',(0.722929908501543,-0.244251601209411,
-0.663382628119203));
#9273=CARTESIAN_POINT('Ctrl Pts',(0.707917883896095,-0.246942143572133,
-0.679352081686668));
#9274=CARTESIAN_POINT('Ctrl Pts',(0.679352081686668,-0.246942143572133,
-0.707917883896095));
#9275=CARTESIAN_POINT('Ctrl Pts',(0.663382628119203,-0.244251601209411,
-0.722929908501543));
#9276=CARTESIAN_POINT('Ctrl Pts',(0.631684198665438,-0.232861760990032,
-0.750785745543687));
#9277=CARTESIAN_POINT('Ctrl Pts',(0.615966552324775,-0.224161999508995,
-0.763642258217232));
#9278=CARTESIAN_POINT('Ctrl Pts',(0.587792702767295,-0.203463743702801,
-0.78555112003688));
#9279=CARTESIAN_POINT('Ctrl Pts',(0.573915184558107,-0.190326085855194,
-0.795684265985088));
#9280=CARTESIAN_POINT('Ctrl Pts',(0.548874290046456,-0.159766064500479,
-0.813159949759));
#9281=CARTESIAN_POINT('Ctrl Pts',(0.537715343527944,-0.142345102874864,
-0.820511285096538));
#9282=CARTESIAN_POINT('Ctrl Pts',(0.517157748491652,-0.099930567888331,
-0.833661031856294));
#9283=CARTESIAN_POINT('Ctrl Pts',(0.508899795931835,-0.0740444353928835,
-0.838633903678357));
#9284=CARTESIAN_POINT('Ctrl Pts',(0.504455939115715,-0.04763,-0.841298510752801));
#9285=CARTESIAN_POINT('Origin',(0.707106781186548,-0.04763,-0.707106781186547));
#9286=CARTESIAN_POINT('Origin',(0.,-0.166705,0.));
#9287=CARTESIAN_POINT('',(-0.980948,-0.28578,1.20131482833E-16));
#9288=CARTESIAN_POINT('Origin',(0.,-0.28578,0.));
#9289=CARTESIAN_POINT('',(-0.980948,-0.166705,1.20131482833E-16));
#9290=CARTESIAN_POINT('',(0.951592097314,-0.04763,0.238183666596899));
#9291=CARTESIAN_POINT('Origin',(0.,-0.04763,0.));
#9292=CARTESIAN_POINT('',(0.951592097314,-0.04763,-0.238183666596899));
#9293=CARTESIAN_POINT('Ctrl Pts',(0.951592097314,-0.04763,0.238183666596899));
#9294=CARTESIAN_POINT('Ctrl Pts',(0.952850216871763,-0.0740444353928835,
0.233157223576062));
#9295=CARTESIAN_POINT('Ctrl Pts',(0.955173119738174,-0.099930567888331,
0.223801617934945));
#9296=CARTESIAN_POINT('Ctrl Pts',(0.960411259488514,-0.142345102874864,
0.199966927975188));
#9297=CARTESIAN_POINT('Ctrl Pts',(0.963103647174702,-0.15976606450048,0.1868781821531));
#9298=CARTESIAN_POINT('Ctrl Pts',(0.968453058988463,-0.190326085855194,
0.15681442133453));
#9299=CARTESIAN_POINT('Ctrl Pts',(0.971100730005489,-0.203463743702801,
0.139836317888042));
#9300=CARTESIAN_POINT('Ctrl Pts',(0.975530745318961,-0.224161999508995,
0.104422493053067));
#9301=CARTESIAN_POINT('Ctrl Pts',(0.977553872336861,-0.232861760990032,
0.0842175114474172));
#9302=CARTESIAN_POINT('Ctrl Pts',(0.980270995488453,-0.244251601209411,
0.0421062857595697));
#9303=CARTESIAN_POINT('Ctrl Pts',(0.980948,-0.246942143572133,0.0201990724523194));
#9304=CARTESIAN_POINT('Ctrl Pts',(0.980948,-0.246942143572133,-0.0201990724523194));
#9305=CARTESIAN_POINT('Ctrl Pts',(0.980270995488453,-0.244251601209411,
-0.0421062857595697));
#9306=CARTESIAN_POINT('Ctrl Pts',(0.977553872336861,-0.232861760990032,
-0.0842175114474172));
#9307=CARTESIAN_POINT('Ctrl Pts',(0.975530745318961,-0.224161999508995,
-0.104422493053067));
#9308=CARTESIAN_POINT('Ctrl Pts',(0.971100730005489,-0.203463743702801,
-0.139836317888042));
#9309=CARTESIAN_POINT('Ctrl Pts',(0.968453058988463,-0.190326085855194,
-0.15681442133453));
#9310=CARTESIAN_POINT('Ctrl Pts',(0.963103647174702,-0.15976606450048,-0.1868781821531));
#9311=CARTESIAN_POINT('Ctrl Pts',(0.960411259488514,-0.142345102874864,
-0.199966927975188));
#9312=CARTESIAN_POINT('Ctrl Pts',(0.955173119738174,-0.099930567888331,
-0.223801617934945));
#9313=CARTESIAN_POINT('Ctrl Pts',(0.952850216871763,-0.0740444353928835,
-0.233157223576062));
#9314=CARTESIAN_POINT('Ctrl Pts',(0.951592097314,-0.0476299999999999,-0.238183666596899));
#9315=CARTESIAN_POINT('Origin',(0.,-0.04763,0.));
#9316=CARTESIAN_POINT('Origin',(0.,-0.04763,0.));
#9317=CARTESIAN_POINT('Origin',(1.,-0.04763,0.));
#9318=CARTESIAN_POINT('Origin',(1.,0.,0.));
#9319=CARTESIAN_POINT('Origin',(1.,-0.04763,0.));
#9320=CARTESIAN_POINT('Origin',(0.,-0.28578,0.));
#9321=CARTESIAN_POINT('Origin',(0.,-0.04763,0.));
#9322=CARTESIAN_POINT('',(0.,0.,0.));
#9323=CARTESIAN_POINT('Origin',(1.013815,0.445,0.));
#9324=CARTESIAN_POINT('',(-1.013815,0.445,-1.24156529467757E-16));
#9325=CARTESIAN_POINT('Origin',(0.,0.445,0.));
#9326=CARTESIAN_POINT('',(-0.991185,0.445,-1.21385153761287E-16));
#9327=CARTESIAN_POINT('Origin',(0.,0.445,0.));
#9328=CARTESIAN_POINT('Origin',(0.,0.4075,0.));
#9329=CARTESIAN_POINT('',(-1.013815,0.37,-1.24156529467757E-16));
#9330=CARTESIAN_POINT('Origin',(0.,0.37,0.));
#9331=CARTESIAN_POINT('',(-1.013815,0.4075,-1.24156529467757E-16));
#9332=CARTESIAN_POINT('Origin',(0.991185,0.37,0.));
#9333=CARTESIAN_POINT('',(-0.991185,0.37,-1.21385153761287E-16));
#9334=CARTESIAN_POINT('Origin',(0.,0.37,0.));
#9335=CARTESIAN_POINT('Origin',(0.,0.4075,0.));
#9336=CARTESIAN_POINT('',(-0.991185,0.4075,-1.21385153761287E-16));
#9337=CARTESIAN_POINT('Origin',(1.013815,-0.37,0.));
#9338=CARTESIAN_POINT('',(-1.013815,-0.37,-1.24156529467757E-16));
#9339=CARTESIAN_POINT('Origin',(0.,-0.37,0.));
#9340=CARTESIAN_POINT('',(-0.991185,-0.37,-1.21385153761287E-16));
#9341=CARTESIAN_POINT('Origin',(0.,-0.37,0.));
#9342=CARTESIAN_POINT('Origin',(0.,-0.4075,0.));
#9343=CARTESIAN_POINT('',(-1.013815,-0.445,-1.24156529467757E-16));
#9344=CARTESIAN_POINT('Origin',(0.,-0.445,0.));
#9345=CARTESIAN_POINT('',(-1.013815,-0.4075,-1.24156529467757E-16));
#9346=CARTESIAN_POINT('Origin',(0.991185,-0.445,0.));
#9347=CARTESIAN_POINT('',(-0.991185,-0.445,-1.21385153761287E-16));
#9348=CARTESIAN_POINT('Origin',(0.,-0.445,0.));
#9349=CARTESIAN_POINT('Origin',(0.,-0.4075,0.));
#9350=CARTESIAN_POINT('',(-0.991185,-0.4075,-1.21385153761287E-16));
#9351=CARTESIAN_POINT('',(0.,0.,0.));
#9352=CARTESIAN_POINT('',(0.,0.,0.));
#9353=CARTESIAN_POINT('',(0.,0.,0.));
#9354=CARTESIAN_POINT('',(0.,0.,0.));
#9355=CARTESIAN_POINT('',(0.,0.,0.));
#9356=CARTESIAN_POINT('',(0.,0.,0.));
#9357=CARTESIAN_POINT('Origin',(0.0866025403784439,-0.4,-0.15));
#9358=CARTESIAN_POINT('',(0.173205080756888,-0.4,0.));
#9359=CARTESIAN_POINT('',(0.0866025403784439,-0.4,-0.15));
#9360=CARTESIAN_POINT('',(0.173205080756888,-0.4,0.));
#9361=CARTESIAN_POINT('',(0.0866025403784439,-0.64,-0.15));
#9362=CARTESIAN_POINT('',(0.0866025403784439,-0.4,-0.15));
#9363=CARTESIAN_POINT('',(0.173205080756888,-0.64,0.));
#9364=CARTESIAN_POINT('',(0.173205080756888,-0.64,0.));
#9365=CARTESIAN_POINT('',(0.173205080756888,-0.4,0.));
#9366=CARTESIAN_POINT('Origin',(-0.0866025403784438,-0.4,-0.15));
#9367=CARTESIAN_POINT('',(-0.0866025403784438,-0.4,-0.15));
#9368=CARTESIAN_POINT('',(0.0866025403784439,-0.4,-0.15));
#9369=CARTESIAN_POINT('',(-0.0866025403784438,-0.64,-0.15));
#9370=CARTESIAN_POINT('',(-0.0866025403784438,-0.4,-0.15));
#9371=CARTESIAN_POINT('',(0.0866025403784439,-0.64,-0.15));
#9372=CARTESIAN_POINT('Origin',(-0.173205080756888,-0.4,-2.77555756156289E-17));
#9373=CARTESIAN_POINT('',(-0.173205080756888,-0.4,-2.12115047744981E-17));
#9374=CARTESIAN_POINT('',(-0.0866025403784438,-0.4,-0.15));
#9375=CARTESIAN_POINT('',(-0.173205080756888,-0.64,-2.77555756156289E-17));
#9376=CARTESIAN_POINT('',(-0.173205080756888,-0.4,-2.12115047744981E-17));
#9377=CARTESIAN_POINT('',(-0.0866025403784438,-0.64,-0.15));
#9378=CARTESIAN_POINT('Origin',(-0.0866025403784439,-0.4,0.15));
#9379=CARTESIAN_POINT('',(-0.0866025403784439,-0.4,0.15));
#9380=CARTESIAN_POINT('',(-0.173205080756888,-0.4,-2.12115047744981E-17));
#9381=CARTESIAN_POINT('',(-0.0866025403784439,-0.64,0.15));
#9382=CARTESIAN_POINT('',(-0.0866025403784439,-0.4,0.15));
#9383=CARTESIAN_POINT('',(-0.173205080756888,-0.64,-2.12115047744981E-17));
#9384=CARTESIAN_POINT('Origin',(0.0866025403784439,-0.4,0.15));
#9385=CARTESIAN_POINT('',(0.0866025403784439,-0.4,0.15));
#9386=CARTESIAN_POINT('',(-0.0866025403784439,-0.4,0.15));
#9387=CARTESIAN_POINT('',(0.0866025403784439,-0.64,0.15));
#9388=CARTESIAN_POINT('',(0.0866025403784439,-0.4,0.15));
#9389=CARTESIAN_POINT('',(-0.0866025403784439,-0.64,0.15));
#9390=CARTESIAN_POINT('Origin',(0.173205080756888,-0.4,0.));
#9391=CARTESIAN_POINT('',(0.0866025403784439,-0.4,0.15));
#9392=CARTESIAN_POINT('',(0.0866025403784439,-0.64,0.15));
#9393=CARTESIAN_POINT('Origin',(0.,-0.4,-2.77555756156289E-17));
#9394=CARTESIAN_POINT('Origin',(0.,-0.64,-2.77555756156289E-17));
#9395=CARTESIAN_POINT('Origin',(0.,-1.,0.));
#9396=CARTESIAN_POINT('',(-0.1954,-1.,2.39295984553393E-17));
#9397=CARTESIAN_POINT('Origin',(0.,-1.,0.));
#9398=CARTESIAN_POINT('Origin',(0.3,0.4,0.));
#9399=CARTESIAN_POINT('',(-0.3,0.4,-3.67394039744206E-17));
#9400=CARTESIAN_POINT('Origin',(0.,0.4,0.));
#9401=CARTESIAN_POINT('Origin',(0.,0.375,0.));
#9402=CARTESIAN_POINT('',(-0.35,0.35,-4.28626379701573E-17));
#9403=CARTESIAN_POINT('Origin',(0.,0.35,0.));
#9404=CARTESIAN_POINT('',(-0.325,0.375,-3.9801020972289E-17));
#9405=CARTESIAN_POINT('Origin',(0.,0.19,0.));
#9406=CARTESIAN_POINT('',(-0.35,0.03,-4.28626379701574E-17));
#9407=CARTESIAN_POINT('Origin',(0.,0.03,0.));
#9408=CARTESIAN_POINT('',(-0.35,0.19,-4.28626379701574E-17));
#9409=CARTESIAN_POINT('Origin',(0.,0.0149999999999999,0.));
#9410=CARTESIAN_POINT('',(-0.32,-3.29597460435593E-17,-3.91886975727153E-17));
#9411=CARTESIAN_POINT('Origin',(0.,0.,0.));
#9412=CARTESIAN_POINT('',(-0.335,0.0149999999999999,-4.10256677714363E-17));
#9413=CARTESIAN_POINT('Origin',(0.22,0.,0.));
#9414=CARTESIAN_POINT('',(-0.22,-6.93889390390723E-18,-2.69422295812418E-17));
#9415=CARTESIAN_POINT('Origin',(0.,0.,0.));
#9416=CARTESIAN_POINT('Origin',(0.,-0.02,0.));
#9417=CARTESIAN_POINT('',(-0.1954,-0.0492,2.39295984553393E-17));
#9418=CARTESIAN_POINT('Origin',(0.,-0.0492,0.));
#9419=CARTESIAN_POINT('',(-0.21,-0.02,-2.57175827820944E-17));
#9420=CARTESIAN_POINT('Origin',(0.,-0.8,0.));
#9421=CARTESIAN_POINT('',(-0.1954,-0.8,-2.39295984553393E-17));
#9422=CARTESIAN_POINT('',(0.,0.,0.));
#9423=CARTESIAN_POINT('',(0.,0.,0.));
#9424=CARTESIAN_POINT('',(0.,0.,0.));
#9425=CARTESIAN_POINT('',(0.,0.,0.));
#9426=CARTESIAN_POINT('',(0.,0.,0.));
#9427=CARTESIAN_POINT('',(0.,0.,0.));
#9428=CARTESIAN_POINT('',(0.,0.,0.));
#9429=CARTESIAN_POINT('',(0.,0.,0.));
#9430=CARTESIAN_POINT('',(0.,0.,0.));
#9431=CARTESIAN_POINT('',(0.,0.,0.));
#9432=CARTESIAN_POINT('',(0.,0.,0.));
#9433=CARTESIAN_POINT('',(0.,0.,0.));
#9434=CARTESIAN_POINT('',(0.,0.,0.));
#9435=CARTESIAN_POINT('',(0.,0.,0.));
#9436=CARTESIAN_POINT('',(0.,0.,0.));
#9437=CARTESIAN_POINT('',(0.,0.,0.));
#9438=CARTESIAN_POINT('',(0.,0.,0.));
#9439=CARTESIAN_POINT('',(-5.3,-1.8,0.8));
#9440=CARTESIAN_POINT('',(-5.3,-1.8,0.96));
#9441=CARTESIAN_POINT('',(-5.3,1.8,0.8));
#9442=CARTESIAN_POINT('',(-5.3,1.8,0.96));
#9443=CARTESIAN_POINT('',(-2.2,-1.8,0.8));
#9444=CARTESIAN_POINT('',(-2.2,-1.8,0.96));
#9445=CARTESIAN_POINT('',(-2.2,1.8,0.8));
#9446=CARTESIAN_POINT('',(-2.2,1.8,0.96));
#9447=CARTESIAN_POINT('',(0.,0.,2.95));
#9448=CARTESIAN_POINT('',(1.75,0.,3.6));
#9449=CARTESIAN_POINT('',(-0.875,1.51554445662277,3.6));
#9450=CARTESIAN_POINT('',(-0.875000000000001,-1.51554445662277,3.6));
#9451=CARTESIAN_POINT('',(0.,0.,11.05));
#9452=CARTESIAN_POINT('',(1.75,0.,10.4));
#9453=CARTESIAN_POINT('',(-0.875,1.51554445662277,10.4));
#9454=CARTESIAN_POINT('',(-0.875000000000001,-1.51554445662277,10.4));
#9455=CARTESIAN_POINT('',(0.,0.,0.));
#9456=CARTESIAN_POINT('',(0.,0.,0.));
#9457=CARTESIAN_POINT('Origin',(0.,0.,10.5));
#9458=CARTESIAN_POINT('',(-0.165,-2.02066721859313E-17,10.5));
#9459=CARTESIAN_POINT('Origin',(0.,0.,10.5));
#9460=CARTESIAN_POINT('',(-0.165,2.02066721859313E-17,12.));
#9461=CARTESIAN_POINT('',(-0.165,-2.02066721859313E-17,10.5));
#9462=CARTESIAN_POINT('Origin',(0.,0.,12.));
#9463=CARTESIAN_POINT('Origin',(0.,0.,10.5));
#9464=CARTESIAN_POINT('Origin',(0.,0.,1.9));
#9465=CARTESIAN_POINT('',(-0.165,-2.02066721859313E-17,2.));
#9466=CARTESIAN_POINT('Origin',(0.,0.,2.));
#9467=CARTESIAN_POINT('',(-0.165,-2.02066721859313E-17,3.5));
#9468=CARTESIAN_POINT('',(-0.165,-2.02066721859313E-17,1.9));
#9469=CARTESIAN_POINT('Origin',(0.,0.,3.5));
#9470=CARTESIAN_POINT('Origin',(0.,0.,3.5));
#9471=CARTESIAN_POINT('Origin',(0.,-2.05,7.2));
#9472=CARTESIAN_POINT('',(0.155246105783993,-1.79329268292683,7.2));
#9473=CARTESIAN_POINT('Ctrl Pts',(0.155246105783993,-1.79329268292683,7.2));
#9474=CARTESIAN_POINT('Ctrl Pts',(0.155246105783993,-1.79329268292683,7.17201748936946));
#9475=CARTESIAN_POINT('Ctrl Pts',(0.148285663496836,-1.79393443972947,7.14272186726396));
#9476=CARTESIAN_POINT('Ctrl Pts',(0.127697249529238,-1.79547787365052,7.1044926805215));
#9477=CARTESIAN_POINT('Ctrl Pts',(0.119189936856738,-1.79607670590828,7.0926589910604));
#9478=CARTESIAN_POINT('Ctrl Pts',(0.0995353781147738,-1.79727260133503,
7.07183236368701));
#9479=CARTESIAN_POINT('Ctrl Pts',(0.08838803635753,-1.7978684994743,7.06283944919615));
#9480=CARTESIAN_POINT('Ctrl Pts',(0.0655526842737879,-1.79883881216911,
7.04906264597394));
#9481=CARTESIAN_POINT('Ctrl Pts',(0.0528849064848421,-1.79927148532923,
7.04338913442002));
#9482=CARTESIAN_POINT('Ctrl Pts',(0.0264570277515568,-1.79985408312092,
7.03594022256534));
#9483=CARTESIAN_POINT('Ctrl Pts',(0.0126957287507039,-1.8,7.03416876048223));
#9484=CARTESIAN_POINT('Ctrl Pts',(-0.0126957287507037,-1.8,7.03416876048223));
#9485=CARTESIAN_POINT('Ctrl Pts',(-0.0264570277515565,-1.79985408312092,
7.03594022256534));
#9486=CARTESIAN_POINT('Ctrl Pts',(-0.0528849064848418,-1.79927148532923,
7.04338913442002));
#9487=CARTESIAN_POINT('Ctrl Pts',(-0.0655526842737877,-1.79883881216911,
7.04906264597394));
#9488=CARTESIAN_POINT('Ctrl Pts',(-0.0883880363575299,-1.7978684994743,
7.06283944919615));
#9489=CARTESIAN_POINT('Ctrl Pts',(-0.0995353781147733,-1.79727260133503,
7.07183236368701));
#9490=CARTESIAN_POINT('Ctrl Pts',(-0.119189936856738,-1.79607670590828,
7.0926589910604));
#9491=CARTESIAN_POINT('Ctrl Pts',(-0.127697249529239,-1.79547787365052,
7.1044926805215));
#9492=CARTESIAN_POINT('Ctrl Pts',(-0.148285663496837,-1.79393443972947,
7.14272186726397));
#9493=CARTESIAN_POINT('Ctrl Pts',(-0.155246105783993,-1.79329268292683,
7.17201748936946));
#9494=CARTESIAN_POINT('Ctrl Pts',(-0.155246105783993,-1.79329268292683,
7.22798251063054));
#9495=CARTESIAN_POINT('Ctrl Pts',(-0.148285663496836,-1.79393443972947,
7.25727813273604));
#9496=CARTESIAN_POINT('Ctrl Pts',(-0.127697249529237,-1.79547787365052,
7.2955073194785));
#9497=CARTESIAN_POINT('Ctrl Pts',(-0.119189936856737,-1.79607670590828,
7.3073410089396));
#9498=CARTESIAN_POINT('Ctrl Pts',(-0.0995353781147728,-1.79727260133503,
7.32816763631299));
#9499=CARTESIAN_POINT('Ctrl Pts',(-0.0883880363575299,-1.7978684994743,
7.33716055080385));
#9500=CARTESIAN_POINT('Ctrl Pts',(-0.0655526842737877,-1.79883881216911,
7.35093735402606));
#9501=CARTESIAN_POINT('Ctrl Pts',(-0.0528849064848417,-1.79927148532923,
7.35661086557998));
#9502=CARTESIAN_POINT('Ctrl Pts',(-0.0264570277515566,-1.79985408312092,
7.36405977743466));
#9503=CARTESIAN_POINT('Ctrl Pts',(-0.0126957287507037,-1.8,7.36583123951777));
#9504=CARTESIAN_POINT('Ctrl Pts',(0.0126957287507039,-1.8,7.36583123951777));
#9505=CARTESIAN_POINT('Ctrl Pts',(0.0264570277515567,-1.79985408312092,
7.36405977743466));
#9506=CARTESIAN_POINT('Ctrl Pts',(0.0528849064848419,-1.79927148532923,
7.35661086557998));
#9507=CARTESIAN_POINT('Ctrl Pts',(0.0655526842737879,-1.79883881216911,
7.35093735402606));
#9508=CARTESIAN_POINT('Ctrl Pts',(0.08838803635753,-1.7978684994743,7.33716055080385));
#9509=CARTESIAN_POINT('Ctrl Pts',(0.0995353781147734,-1.79727260133503,
7.32816763631299));
#9510=CARTESIAN_POINT('Ctrl Pts',(0.119189936856738,-1.79607670590828,7.3073410089396));
#9511=CARTESIAN_POINT('Ctrl Pts',(0.127697249529238,-1.79547787365052,7.2955073194785));
#9512=CARTESIAN_POINT('Ctrl Pts',(0.148285663496836,-1.79393443972947,7.25727813273604));
#9513=CARTESIAN_POINT('Ctrl Pts',(0.155246105783993,-1.79329268292683,7.22798251063054));
#9514=CARTESIAN_POINT('Ctrl Pts',(0.155246105783993,-1.79329268292683,7.2));
#9515=CARTESIAN_POINT('Origin',(0.,0.,7.6));
#9516=CARTESIAN_POINT('',(0.953939201416946,-0.3,7.6));
#9517=CARTESIAN_POINT('',(1.77482393492988,-0.3,7.6));
#9518=CARTESIAN_POINT('',(0.4,-0.3,7.6));
#9519=CARTESIAN_POINT('',(0.953939201416946,0.3,7.6));
#9520=CARTESIAN_POINT('Origin',(0.,0.,7.6));
#9521=CARTESIAN_POINT('',(1.77482393492988,0.3,7.6));
#9522=CARTESIAN_POINT('',(5.4,0.3,7.6));
#9523=CARTESIAN_POINT('Origin',(0.,0.,7.6));
#9524=CARTESIAN_POINT('Origin',(0.,0.,6.8));
#9525=CARTESIAN_POINT('',(1.77482393492988,-0.3,6.8));
#9526=CARTESIAN_POINT('',(1.77482393492988,-0.3,6.8));
#9527=CARTESIAN_POINT('',(1.77482393492988,0.3,6.8));
#9528=CARTESIAN_POINT('',(1.77482393492988,0.3,6.8));
#9529=CARTESIAN_POINT('Origin',(0.,0.,6.8));
#9530=CARTESIAN_POINT('Origin',(0.,0.,6.8));
#9531=CARTESIAN_POINT('',(0.953939201416946,-0.3,6.8));
#9532=CARTESIAN_POINT('',(0.4,-0.3,6.8));
#9533=CARTESIAN_POINT('',(0.953939201416946,0.3,6.8));
#9534=CARTESIAN_POINT('',(5.4,0.3,6.8));
#9535=CARTESIAN_POINT('Origin',(0.,0.,6.8));
#9536=CARTESIAN_POINT('Origin',(0.8,-0.3,4.));
#9537=CARTESIAN_POINT('',(0.953939201416946,-0.3,4.));
#9538=CARTESIAN_POINT('',(0.953939201416946,-0.3,4.));
#9539=CARTESIAN_POINT('',(10.8,-0.3,4.));
#9540=CARTESIAN_POINT('',(0.8,-0.3,4.));
#9541=CARTESIAN_POINT('',(10.8,-0.3,10.));
#9542=CARTESIAN_POINT('',(10.8,-0.3,4.));
#9543=CARTESIAN_POINT('',(0.953939201416946,-0.3,10.));
#9544=CARTESIAN_POINT('',(0.8,-0.3,10.));
#9545=CARTESIAN_POINT('',(0.953939201416946,-0.3,4.));
#9546=CARTESIAN_POINT('',(8.47,-0.3,8.5));
#9547=CARTESIAN_POINT('Origin',(8.8,-0.3,8.5));
#9548=CARTESIAN_POINT('',(2.47,-0.3,5.5));
#9549=CARTESIAN_POINT('Origin',(2.8,-0.3,5.5));
#9550=CARTESIAN_POINT('',(2.47,-0.3,8.5));
#9551=CARTESIAN_POINT('Origin',(2.8,-0.3,8.5));
#9552=CARTESIAN_POINT('',(8.47,-0.3,5.5));
#9553=CARTESIAN_POINT('Origin',(8.8,-0.3,5.5));
#9554=CARTESIAN_POINT('Origin',(0.,0.,4.));
#9555=CARTESIAN_POINT('',(0.953939201416946,0.3,4.));
#9556=CARTESIAN_POINT('',(0.953939201416946,0.3,4.));
#9557=CARTESIAN_POINT('Origin',(0.,0.,4.));
#9558=CARTESIAN_POINT('Origin',(8.8,-0.4,5.5));
#9559=CARTESIAN_POINT('',(8.47,0.3,5.5));
#9560=CARTESIAN_POINT('',(8.47,-0.4,5.5));
#9561=CARTESIAN_POINT('Origin',(8.8,0.3,5.5));
#9562=CARTESIAN_POINT('Origin',(2.8,-0.4,8.5));
#9563=CARTESIAN_POINT('',(2.47,0.3,8.5));
#9564=CARTESIAN_POINT('',(2.47,-0.4,8.5));
#9565=CARTESIAN_POINT('Origin',(2.8,0.3,8.5));
#9566=CARTESIAN_POINT('Origin',(2.8,-0.4,5.5));
#9567=CARTESIAN_POINT('',(2.47,0.3,5.5));
#9568=CARTESIAN_POINT('',(2.47,-0.4,5.5));
#9569=CARTESIAN_POINT('Origin',(2.8,0.3,5.5));
#9570=CARTESIAN_POINT('Origin',(8.8,-0.4,8.5));
#9571=CARTESIAN_POINT('',(8.47,0.3,8.5));
#9572=CARTESIAN_POINT('',(8.47,-0.4,8.5));
#9573=CARTESIAN_POINT('Origin',(8.8,0.3,8.5));
#9574=CARTESIAN_POINT('Origin',(10.8,0.3,4.));
#9575=CARTESIAN_POINT('',(0.953939201416946,0.3,10.));
#9576=CARTESIAN_POINT('',(0.953939201416946,0.3,4.));
#9577=CARTESIAN_POINT('',(10.8,0.3,10.));
#9578=CARTESIAN_POINT('',(10.8,0.3,10.));
#9579=CARTESIAN_POINT('',(10.8,0.3,4.));
#9580=CARTESIAN_POINT('',(10.8,0.3,4.));
#9581=CARTESIAN_POINT('',(10.8,0.3,4.));
#9582=CARTESIAN_POINT('Origin',(10.8,-0.3,4.));
#9583=CARTESIAN_POINT('',(10.8,-0.3,4.));
#9584=CARTESIAN_POINT('',(10.8,-0.3,10.));
#9585=CARTESIAN_POINT('Origin',(0.,0.,4.));
#9586=CARTESIAN_POINT('Origin',(0.,0.,10.));
#9587=CARTESIAN_POINT('Origin',(0.,0.,4.));
#9588=CARTESIAN_POINT('',(-0.5,6.12323399573677E-17,4.));
#9589=CARTESIAN_POINT('Origin',(0.,0.,4.));
#9590=CARTESIAN_POINT('Origin',(0.,0.,10.));
#9591=CARTESIAN_POINT('',(-0.5,-6.12323399573677E-17,10.));
#9592=CARTESIAN_POINT('Origin',(0.,0.,10.));
#9593=CARTESIAN_POINT('Origin',(0.,0.,2.));
#9594=CARTESIAN_POINT('',(-0.5,-6.12323399573677E-17,2.));
#9595=CARTESIAN_POINT('',(-0.5,-6.12323399573677E-17,2.));
#9596=CARTESIAN_POINT('Origin',(0.,0.,2.));
#9597=CARTESIAN_POINT('Origin',(0.,0.,2.));
#9598=CARTESIAN_POINT('',(-0.5,-6.12323399573677E-17,12.));
#9599=CARTESIAN_POINT('Origin',(0.,0.,12.));
#9600=CARTESIAN_POINT('',(-0.5,-6.12323399573677E-17,2.));
#9601=CARTESIAN_POINT('Origin',(0.,0.,12.));
#9602=CARTESIAN_POINT('Origin',(0.,0.,2.));
#9603=CARTESIAN_POINT('',(0.,0.,0.));
#9604=CARTESIAN_POINT('Origin',(0.,0.,3.4));
#9605=CARTESIAN_POINT('',(-0.505,-6.18446633569413E-17,4.));
#9606=CARTESIAN_POINT('Origin',(0.,0.,4.));
#9607=CARTESIAN_POINT('',(-0.505,-6.18446633569413E-17,3.4));
#9608=CARTESIAN_POINT('',(-0.505,-6.18446633569413E-17,3.4));
#9609=CARTESIAN_POINT('Origin',(0.,0.,3.4));
#9610=CARTESIAN_POINT('Origin',(0.,0.,3.4));
#9611=CARTESIAN_POINT('',(-0.7,-8.57252759403147E-17,4.));
#9612=CARTESIAN_POINT('Origin',(0.,0.,4.));
#9613=CARTESIAN_POINT('',(-0.7,-8.57252759403147E-17,3.4));
#9614=CARTESIAN_POINT('',(-0.7,-8.57252759403147E-17,3.4));
#9615=CARTESIAN_POINT('Origin',(0.,0.,3.4));
#9616=CARTESIAN_POINT('Origin',(0.,0.,4.));
#9617=CARTESIAN_POINT('Origin',(0.,0.,3.4));
#9618=CARTESIAN_POINT('',(0.,0.,0.));
#9619=CARTESIAN_POINT('Origin',(0.,0.,10.));
#9620=CARTESIAN_POINT('',(-0.505,-6.18446633569413E-17,10.6));
#9621=CARTESIAN_POINT('Origin',(0.,0.,10.6));
#9622=CARTESIAN_POINT('',(-0.505,-6.18446633569413E-17,10.));
#9623=CARTESIAN_POINT('',(-0.505,-6.18446633569413E-17,10.));
#9624=CARTESIAN_POINT('Origin',(0.,0.,10.));
#9625=CARTESIAN_POINT('Origin',(0.,0.,10.));
#9626=CARTESIAN_POINT('',(-0.7,-8.57252759403147E-17,10.6));
#9627=CARTESIAN_POINT('Origin',(0.,0.,10.6));
#9628=CARTESIAN_POINT('',(-0.7,-8.57252759403147E-17,10.));
#9629=CARTESIAN_POINT('',(-0.7,-8.57252759403147E-17,10.));
#9630=CARTESIAN_POINT('Origin',(0.,0.,10.));
#9631=CARTESIAN_POINT('Origin',(0.,0.,10.6));
#9632=CARTESIAN_POINT('Origin',(0.,0.,10.));
#9633=CARTESIAN_POINT('',(0.,0.,0.));
#9634=CARTESIAN_POINT('Origin',(0.,0.,1.8));
#9635=CARTESIAN_POINT('',(-0.225,-2.75545529808154E-17,2.));
#9636=CARTESIAN_POINT('Origin',(0.,0.,2.));
#9637=CARTESIAN_POINT('',(-0.225,-2.75545529808154E-17,1.8));
#9638=CARTESIAN_POINT('',(-0.225,-2.75545529808154E-17,1.8));
#9639=CARTESIAN_POINT('Origin',(0.,0.,1.8));
#9640=CARTESIAN_POINT('Origin',(0.,0.,1.8));
#9641=CARTESIAN_POINT('',(-0.9,-1.10218211923262E-16,2.));
#9642=CARTESIAN_POINT('Origin',(0.,0.,2.));
#9643=CARTESIAN_POINT('',(-0.9,-1.10218211923262E-16,1.8));
#9644=CARTESIAN_POINT('',(-0.9,-1.10218211923262E-16,1.8));
#9645=CARTESIAN_POINT('Origin',(0.,0.,1.8));
#9646=CARTESIAN_POINT('Origin',(0.,0.,2.));
#9647=CARTESIAN_POINT('Origin',(0.,0.,1.8));
#9648=CARTESIAN_POINT('',(0.,0.,0.));
#9649=CARTESIAN_POINT('Origin',(0.,0.,12.));
#9650=CARTESIAN_POINT('',(-0.225,-2.75545529808154E-17,12.2));
#9651=CARTESIAN_POINT('Origin',(0.,0.,12.2));
#9652=CARTESIAN_POINT('',(-0.225,-2.75545529808154E-17,12.));
#9653=CARTESIAN_POINT('',(-0.225,-2.75545529808154E-17,12.));
#9654=CARTESIAN_POINT('Origin',(0.,0.,12.));
#9655=CARTESIAN_POINT('Origin',(0.,0.,12.));
#9656=CARTESIAN_POINT('',(-0.9,-1.10218211923262E-16,12.2));
#9657=CARTESIAN_POINT('Origin',(0.,0.,12.2));
#9658=CARTESIAN_POINT('',(-0.9,-1.10218211923262E-16,12.));
#9659=CARTESIAN_POINT('',(-0.9,-1.10218211923262E-16,12.));
#9660=CARTESIAN_POINT('Origin',(0.,0.,12.));
#9661=CARTESIAN_POINT('Origin',(0.,0.,12.2));
#9662=CARTESIAN_POINT('Origin',(0.,0.,12.));
#9663=CARTESIAN_POINT('',(0.,0.,0.));
#9664=CARTESIAN_POINT('Origin',(0.3,0.4,0.));
#9665=CARTESIAN_POINT('',(-0.3,0.4,-3.67394039744206E-17));
#9666=CARTESIAN_POINT('Origin',(0.,0.4,0.));
#9667=CARTESIAN_POINT('Origin',(0.,0.375,0.));
#9668=CARTESIAN_POINT('',(-0.35,0.35,-4.28626379701573E-17));
#9669=CARTESIAN_POINT('Origin',(0.,0.35,0.));
#9670=CARTESIAN_POINT('',(-0.325,0.375,-3.9801020972289E-17));
#9671=CARTESIAN_POINT('Origin',(0.,0.19,0.));
#9672=CARTESIAN_POINT('',(-0.35,0.03,-4.28626379701574E-17));
#9673=CARTESIAN_POINT('Origin',(0.,0.03,0.));
#9674=CARTESIAN_POINT('',(-0.35,0.19,-4.28626379701574E-17));
#9675=CARTESIAN_POINT('Origin',(0.,0.0149999999999999,0.));
#9676=CARTESIAN_POINT('',(-0.32,-3.29597460435593E-17,-3.91886975727153E-17));
#9677=CARTESIAN_POINT('Origin',(0.,0.,0.));
#9678=CARTESIAN_POINT('',(-0.335,0.0149999999999999,-4.10256677714363E-17));
#9679=CARTESIAN_POINT('Origin',(0.22,0.,0.));
#9680=CARTESIAN_POINT('',(-0.22,-6.93889390390723E-18,-2.69422295812418E-17));
#9681=CARTESIAN_POINT('Origin',(0.,0.,0.));
#9682=CARTESIAN_POINT('Origin',(0.,-0.02,0.));
#9683=CARTESIAN_POINT('',(-0.1954,-0.0492,2.39295984553393E-17));
#9684=CARTESIAN_POINT('Origin',(0.,-0.0492,0.));
#9685=CARTESIAN_POINT('',(-0.21,-0.02,-2.57175827820944E-17));
#9686=CARTESIAN_POINT('Origin',(0.,-0.8,0.));
#9687=CARTESIAN_POINT('',(-0.1954,-1.5646,2.39295984553393E-17));
#9688=CARTESIAN_POINT('Origin',(0.,-1.5646,0.));
#9689=CARTESIAN_POINT('',(-0.1954,-0.8,-2.39295984553393E-17));
#9690=CARTESIAN_POINT('Origin',(0.,-1.58,0.));
#9691=CARTESIAN_POINT('',(-0.16,-1.6,-1.95943487863577E-17));
#9692=CARTESIAN_POINT('Origin',(0.,-1.6,0.));
#9693=CARTESIAN_POINT('',(-0.18,-1.58,-2.20436423846524E-17));
#9694=CARTESIAN_POINT('Origin',(0.,-1.6,0.));
#9695=CARTESIAN_POINT('Origin',(0.0866025403784439,-0.4,-0.15));
#9696=CARTESIAN_POINT('',(0.173205080756888,-0.4,0.));
#9697=CARTESIAN_POINT('',(0.0866025403784439,-0.4,-0.15));
#9698=CARTESIAN_POINT('',(0.173205080756888,-0.4,0.));
#9699=CARTESIAN_POINT('',(0.0866025403784439,-0.64,-0.15));
#9700=CARTESIAN_POINT('',(0.0866025403784439,-0.4,-0.15));
#9701=CARTESIAN_POINT('',(0.173205080756888,-0.64,0.));
#9702=CARTESIAN_POINT('',(0.173205080756888,-0.64,0.));
#9703=CARTESIAN_POINT('',(0.173205080756888,-0.4,0.));
#9704=CARTESIAN_POINT('Origin',(-0.0866025403784438,-0.4,-0.15));
#9705=CARTESIAN_POINT('',(-0.0866025403784438,-0.4,-0.15));
#9706=CARTESIAN_POINT('',(0.0866025403784439,-0.4,-0.15));
#9707=CARTESIAN_POINT('',(-0.0866025403784438,-0.64,-0.15));
#9708=CARTESIAN_POINT('',(-0.0866025403784438,-0.4,-0.15));
#9709=CARTESIAN_POINT('',(0.0866025403784439,-0.64,-0.15));
#9710=CARTESIAN_POINT('Origin',(-0.173205080756888,-0.4,-2.77555756156289E-17));
#9711=CARTESIAN_POINT('',(-0.173205080756888,-0.4,-2.12115047744981E-17));
#9712=CARTESIAN_POINT('',(-0.0866025403784438,-0.4,-0.15));
#9713=CARTESIAN_POINT('',(-0.173205080756888,-0.64,-2.77555756156289E-17));
#9714=CARTESIAN_POINT('',(-0.173205080756888,-0.4,-2.12115047744981E-17));
#9715=CARTESIAN_POINT('',(-0.0866025403784438,-0.64,-0.15));
#9716=CARTESIAN_POINT('Origin',(-0.0866025403784439,-0.4,0.15));
#9717=CARTESIAN_POINT('',(-0.0866025403784439,-0.4,0.15));
#9718=CARTESIAN_POINT('',(-0.173205080756888,-0.4,-2.12115047744981E-17));
#9719=CARTESIAN_POINT('',(-0.0866025403784439,-0.64,0.15));
#9720=CARTESIAN_POINT('',(-0.0866025403784439,-0.4,0.15));
#9721=CARTESIAN_POINT('',(-0.173205080756888,-0.64,-2.12115047744981E-17));
#9722=CARTESIAN_POINT('Origin',(0.0866025403784439,-0.4,0.15));
#9723=CARTESIAN_POINT('',(0.0866025403784439,-0.4,0.15));
#9724=CARTESIAN_POINT('',(-0.0866025403784439,-0.4,0.15));
#9725=CARTESIAN_POINT('',(0.0866025403784439,-0.64,0.15));
#9726=CARTESIAN_POINT('',(0.0866025403784439,-0.4,0.15));
#9727=CARTESIAN_POINT('',(-0.0866025403784439,-0.64,0.15));
#9728=CARTESIAN_POINT('Origin',(0.173205080756888,-0.4,0.));
#9729=CARTESIAN_POINT('',(0.0866025403784439,-0.4,0.15));
#9730=CARTESIAN_POINT('',(0.0866025403784439,-0.64,0.15));
#9731=CARTESIAN_POINT('Origin',(0.,-0.4,-2.77555756156289E-17));
#9732=CARTESIAN_POINT('Origin',(0.,-0.64,-2.77555756156289E-17));
#9733=CARTESIAN_POINT('',(0.,0.,0.));
#9734=CARTESIAN_POINT('',(0.,0.,0.));
#9735=CARTESIAN_POINT('',(0.,0.,0.));
#9736=CARTESIAN_POINT('',(0.,0.,0.));
#9737=CARTESIAN_POINT('',(0.,0.,0.));
#9738=CARTESIAN_POINT('',(0.,0.,1.8));
#9739=CARTESIAN_POINT('',(0.,0.,12.2));
#9740=CARTESIAN_POINT('',(0.,0.,0.));
#9741=CARTESIAN_POINT('',(0.,0.,0.));
#9742=UNCERTAINTY_MEASURE_WITH_UNIT(LENGTH_MEASURE(0.001),#9814,
'DISTANCE_ACCURACY_VALUE',
'Maximum model space distance between geometric entities at asserted c
onnectivities');
#9743=UNCERTAINTY_MEASURE_WITH_UNIT(LENGTH_MEASURE(0.001),#9814,
'DISTANCE_ACCURACY_VALUE',
'Maximum model space distance between geometric entities at asserted c
onnectivities');
#9744=UNCERTAINTY_MEASURE_WITH_UNIT(LENGTH_MEASURE(0.001),#9814,
'DISTANCE_ACCURACY_VALUE',
'Maximum model space distance between geometric entities at asserted c
onnectivities');
#9745=UNCERTAINTY_MEASURE_WITH_UNIT(LENGTH_MEASURE(0.001),#9814,
'DISTANCE_ACCURACY_VALUE',
'Maximum model space distance between geometric entities at asserted c
onnectivities');
#9746=UNCERTAINTY_MEASURE_WITH_UNIT(LENGTH_MEASURE(0.001),#9814,
'DISTANCE_ACCURACY_VALUE',
'Maximum model space distance between geometric entities at asserted c
onnectivities');
#9747=UNCERTAINTY_MEASURE_WITH_UNIT(LENGTH_MEASURE(0.001),#9814,
'DISTANCE_ACCURACY_VALUE',
'Maximum model space distance between geometric entities at asserted c
onnectivities');
#9748=UNCERTAINTY_MEASURE_WITH_UNIT(LENGTH_MEASURE(0.001),#9814,
'DISTANCE_ACCURACY_VALUE',
'Maximum model space distance between geometric entities at asserted c
onnectivities');
#9749=UNCERTAINTY_MEASURE_WITH_UNIT(LENGTH_MEASURE(0.001),#9814,
'DISTANCE_ACCURACY_VALUE',
'Maximum model space distance between geometric entities at asserted c
onnectivities');
#9750=UNCERTAINTY_MEASURE_WITH_UNIT(LENGTH_MEASURE(0.001),#9814,
'DISTANCE_ACCURACY_VALUE',
'Maximum model space distance between geometric entities at asserted c
onnectivities');
#9751=UNCERTAINTY_MEASURE_WITH_UNIT(LENGTH_MEASURE(0.001),#9814,
'DISTANCE_ACCURACY_VALUE',
'Maximum model space distance between geometric entities at asserted c
onnectivities');
#9752=UNCERTAINTY_MEASURE_WITH_UNIT(LENGTH_MEASURE(0.001),#9814,
'DISTANCE_ACCURACY_VALUE',
'Maximum model space distance between geometric entities at asserted c
onnectivities');
#9753=UNCERTAINTY_MEASURE_WITH_UNIT(LENGTH_MEASURE(0.001),#9814,
'DISTANCE_ACCURACY_VALUE',
'Maximum model space distance between geometric entities at asserted c
onnectivities');
#9754=UNCERTAINTY_MEASURE_WITH_UNIT(LENGTH_MEASURE(0.001),#9814,
'DISTANCE_ACCURACY_VALUE',
'Maximum model space distance between geometric entities at asserted c
onnectivities');
#9755=UNCERTAINTY_MEASURE_WITH_UNIT(LENGTH_MEASURE(0.001),#9814,
'DISTANCE_ACCURACY_VALUE',
'Maximum model space distance between geometric entities at asserted c
onnectivities');
#9756=UNCERTAINTY_MEASURE_WITH_UNIT(LENGTH_MEASURE(0.001),#9814,
'DISTANCE_ACCURACY_VALUE',
'Maximum model space distance between geometric entities at asserted c
onnectivities');
#9757=UNCERTAINTY_MEASURE_WITH_UNIT(LENGTH_MEASURE(0.001),#9814,
'DISTANCE_ACCURACY_VALUE',
'Maximum model space distance between geometric entities at asserted c
onnectivities');
#9758=UNCERTAINTY_MEASURE_WITH_UNIT(LENGTH_MEASURE(0.001),#9814,
'DISTANCE_ACCURACY_VALUE',
'Maximum model space distance between geometric entities at asserted c
onnectivities');
#9759=UNCERTAINTY_MEASURE_WITH_UNIT(LENGTH_MEASURE(0.001),#9814,
'DISTANCE_ACCURACY_VALUE',
'Maximum model space distance between geometric entities at asserted c
onnectivities');
#9760=UNCERTAINTY_MEASURE_WITH_UNIT(LENGTH_MEASURE(0.001),#9814,
'DISTANCE_ACCURACY_VALUE',
'Maximum model space distance between geometric entities at asserted c
onnectivities');
#9761=UNCERTAINTY_MEASURE_WITH_UNIT(LENGTH_MEASURE(0.001),#9814,
'DISTANCE_ACCURACY_VALUE',
'Maximum model space distance between geometric entities at asserted c
onnectivities');
#9762=UNCERTAINTY_MEASURE_WITH_UNIT(LENGTH_MEASURE(0.001),#9814,
'DISTANCE_ACCURACY_VALUE',
'Maximum model space distance between geometric entities at asserted c
onnectivities');
#9763=UNCERTAINTY_MEASURE_WITH_UNIT(LENGTH_MEASURE(0.001),#9814,
'DISTANCE_ACCURACY_VALUE',
'Maximum model space distance between geometric entities at asserted c
onnectivities');
#9764=UNCERTAINTY_MEASURE_WITH_UNIT(LENGTH_MEASURE(0.001),#9814,
'DISTANCE_ACCURACY_VALUE',
'Maximum model space distance between geometric entities at asserted c
onnectivities');
#9765=UNCERTAINTY_MEASURE_WITH_UNIT(LENGTH_MEASURE(0.001),#9814,
'DISTANCE_ACCURACY_VALUE',
'Maximum model space distance between geometric entities at asserted c
onnectivities');
#9766=UNCERTAINTY_MEASURE_WITH_UNIT(LENGTH_MEASURE(0.001),#9814,
'DISTANCE_ACCURACY_VALUE',
'Maximum model space distance between geometric entities at asserted c
onnectivities');
#9767=UNCERTAINTY_MEASURE_WITH_UNIT(LENGTH_MEASURE(0.001),#9814,
'DISTANCE_ACCURACY_VALUE',
'Maximum model space distance between geometric entities at asserted c
onnectivities');
#9768=UNCERTAINTY_MEASURE_WITH_UNIT(LENGTH_MEASURE(0.001),#9814,
'DISTANCE_ACCURACY_VALUE',
'Maximum model space distance between geometric entities at asserted c
onnectivities');
#9769=UNCERTAINTY_MEASURE_WITH_UNIT(LENGTH_MEASURE(0.001),#9814,
'DISTANCE_ACCURACY_VALUE',
'Maximum model space distance between geometric entities at asserted c
onnectivities');
#9770=UNCERTAINTY_MEASURE_WITH_UNIT(LENGTH_MEASURE(0.001),#9814,
'DISTANCE_ACCURACY_VALUE',
'Maximum model space distance between geometric entities at asserted c
onnectivities');
#9771=UNCERTAINTY_MEASURE_WITH_UNIT(LENGTH_MEASURE(0.001),#9814,
'DISTANCE_ACCURACY_VALUE',
'Maximum model space distance between geometric entities at asserted c
onnectivities');
#9772=UNCERTAINTY_MEASURE_WITH_UNIT(LENGTH_MEASURE(0.001),#9814,
'DISTANCE_ACCURACY_VALUE',
'Maximum model space distance between geometric entities at asserted c
onnectivities');
#9773=UNCERTAINTY_MEASURE_WITH_UNIT(LENGTH_MEASURE(0.001),#9814,
'DISTANCE_ACCURACY_VALUE',
'Maximum model space distance between geometric entities at asserted c
onnectivities');
#9774=UNCERTAINTY_MEASURE_WITH_UNIT(LENGTH_MEASURE(0.001),#9814,
'DISTANCE_ACCURACY_VALUE',
'Maximum model space distance between geometric entities at asserted c
onnectivities');
#9775=UNCERTAINTY_MEASURE_WITH_UNIT(LENGTH_MEASURE(0.001),#9814,
'DISTANCE_ACCURACY_VALUE',
'Maximum model space distance between geometric entities at asserted c
onnectivities');
#9776=UNCERTAINTY_MEASURE_WITH_UNIT(LENGTH_MEASURE(0.001),#9814,
'DISTANCE_ACCURACY_VALUE',
'Maximum model space distance between geometric entities at asserted c
onnectivities');
#9777=UNCERTAINTY_MEASURE_WITH_UNIT(LENGTH_MEASURE(0.001),#9814,
'DISTANCE_ACCURACY_VALUE',
'Maximum model space distance between geometric entities at asserted c
onnectivities');
#9778=(
GEOMETRIC_REPRESENTATION_CONTEXT(3)
GLOBAL_UNCERTAINTY_ASSIGNED_CONTEXT((#9742))
GLOBAL_UNIT_ASSIGNED_CONTEXT((#9814,#9816,#9817))
REPRESENTATION_CONTEXT('','3D')
);
#9779=(
GEOMETRIC_REPRESENTATION_CONTEXT(3)
GLOBAL_UNCERTAINTY_ASSIGNED_CONTEXT((#9743))
GLOBAL_UNIT_ASSIGNED_CONTEXT((#9814,#9816,#9817))
REPRESENTATION_CONTEXT('','3D')
);
#9780=(
GEOMETRIC_REPRESENTATION_CONTEXT(3)
GLOBAL_UNCERTAINTY_ASSIGNED_CONTEXT((#9744))
GLOBAL_UNIT_ASSIGNED_CONTEXT((#9814,#9816,#9817))
REPRESENTATION_CONTEXT('','3D')
);
#9781=(
GEOMETRIC_REPRESENTATION_CONTEXT(3)
GLOBAL_UNCERTAINTY_ASSIGNED_CONTEXT((#9745))
GLOBAL_UNIT_ASSIGNED_CONTEXT((#9814,#9816,#9817))
REPRESENTATION_CONTEXT('','3D')
);
#9782=(
GEOMETRIC_REPRESENTATION_CONTEXT(3)
GLOBAL_UNCERTAINTY_ASSIGNED_CONTEXT((#9746))
GLOBAL_UNIT_ASSIGNED_CONTEXT((#9814,#9816,#9817))
REPRESENTATION_CONTEXT('','3D')
);
#9783=(
GEOMETRIC_REPRESENTATION_CONTEXT(3)
GLOBAL_UNCERTAINTY_ASSIGNED_CONTEXT((#9747))
GLOBAL_UNIT_ASSIGNED_CONTEXT((#9814,#9816,#9817))
REPRESENTATION_CONTEXT('','3D')
);
#9784=(
GEOMETRIC_REPRESENTATION_CONTEXT(3)
GLOBAL_UNCERTAINTY_ASSIGNED_CONTEXT((#9748))
GLOBAL_UNIT_ASSIGNED_CONTEXT((#9814,#9816,#9817))
REPRESENTATION_CONTEXT('','3D')
);
#9785=(
GEOMETRIC_REPRESENTATION_CONTEXT(3)
GLOBAL_UNCERTAINTY_ASSIGNED_CONTEXT((#9749))
GLOBAL_UNIT_ASSIGNED_CONTEXT((#9814,#9816,#9817))
REPRESENTATION_CONTEXT('','3D')
);
#9786=(
GEOMETRIC_REPRESENTATION_CONTEXT(3)
GLOBAL_UNCERTAINTY_ASSIGNED_CONTEXT((#9750))
GLOBAL_UNIT_ASSIGNED_CONTEXT((#9814,#9816,#9817))
REPRESENTATION_CONTEXT('','3D')
);
#9787=(
GEOMETRIC_REPRESENTATION_CONTEXT(3)
GLOBAL_UNCERTAINTY_ASSIGNED_CONTEXT((#9751))
GLOBAL_UNIT_ASSIGNED_CONTEXT((#9814,#9816,#9817))
REPRESENTATION_CONTEXT('','3D')
);
#9788=(
GEOMETRIC_REPRESENTATION_CONTEXT(3)
GLOBAL_UNCERTAINTY_ASSIGNED_CONTEXT((#9752))
GLOBAL_UNIT_ASSIGNED_CONTEXT((#9814,#9816,#9817))
REPRESENTATION_CONTEXT('','3D')
);
#9789=(
GEOMETRIC_REPRESENTATION_CONTEXT(3)
GLOBAL_UNCERTAINTY_ASSIGNED_CONTEXT((#9753))
GLOBAL_UNIT_ASSIGNED_CONTEXT((#9814,#9816,#9817))
REPRESENTATION_CONTEXT('','3D')
);
#9790=(
GEOMETRIC_REPRESENTATION_CONTEXT(3)
GLOBAL_UNCERTAINTY_ASSIGNED_CONTEXT((#9754))
GLOBAL_UNIT_ASSIGNED_CONTEXT((#9814,#9816,#9817))
REPRESENTATION_CONTEXT('','3D')
);
#9791=(
GEOMETRIC_REPRESENTATION_CONTEXT(3)
GLOBAL_UNCERTAINTY_ASSIGNED_CONTEXT((#9755))
GLOBAL_UNIT_ASSIGNED_CONTEXT((#9814,#9816,#9817))
REPRESENTATION_CONTEXT('','3D')
);
#9792=(
GEOMETRIC_REPRESENTATION_CONTEXT(3)
GLOBAL_UNCERTAINTY_ASSIGNED_CONTEXT((#9756))
GLOBAL_UNIT_ASSIGNED_CONTEXT((#9814,#9816,#9817))
REPRESENTATION_CONTEXT('','3D')
);
#9793=(
GEOMETRIC_REPRESENTATION_CONTEXT(3)
GLOBAL_UNCERTAINTY_ASSIGNED_CONTEXT((#9757))
GLOBAL_UNIT_ASSIGNED_CONTEXT((#9814,#9816,#9817))
REPRESENTATION_CONTEXT('','3D')
);
#9794=(
GEOMETRIC_REPRESENTATION_CONTEXT(3)
GLOBAL_UNCERTAINTY_ASSIGNED_CONTEXT((#9758))
GLOBAL_UNIT_ASSIGNED_CONTEXT((#9814,#9816,#9817))
REPRESENTATION_CONTEXT('','3D')
);
#9795=(
GEOMETRIC_REPRESENTATION_CONTEXT(3)
GLOBAL_UNCERTAINTY_ASSIGNED_CONTEXT((#9759))
GLOBAL_UNIT_ASSIGNED_CONTEXT((#9814,#9816,#9817))
REPRESENTATION_CONTEXT('','3D')
);
#9796=(
GEOMETRIC_REPRESENTATION_CONTEXT(3)
GLOBAL_UNCERTAINTY_ASSIGNED_CONTEXT((#9760))
GLOBAL_UNIT_ASSIGNED_CONTEXT((#9814,#9816,#9817))
REPRESENTATION_CONTEXT('','3D')
);
#9797=(
GEOMETRIC_REPRESENTATION_CONTEXT(3)
GLOBAL_UNCERTAINTY_ASSIGNED_CONTEXT((#9761))
GLOBAL_UNIT_ASSIGNED_CONTEXT((#9814,#9816,#9817))
REPRESENTATION_CONTEXT('','3D')
);
#9798=(
GEOMETRIC_REPRESENTATION_CONTEXT(3)
GLOBAL_UNCERTAINTY_ASSIGNED_CONTEXT((#9762))
GLOBAL_UNIT_ASSIGNED_CONTEXT((#9814,#9816,#9817))
REPRESENTATION_CONTEXT('','3D')
);
#9799=(
GEOMETRIC_REPRESENTATION_CONTEXT(3)
GLOBAL_UNCERTAINTY_ASSIGNED_CONTEXT((#9763))
GLOBAL_UNIT_ASSIGNED_CONTEXT((#9814,#9816,#9817))
REPRESENTATION_CONTEXT('','3D')
);
#9800=(
GEOMETRIC_REPRESENTATION_CONTEXT(3)
GLOBAL_UNCERTAINTY_ASSIGNED_CONTEXT((#9764))
GLOBAL_UNIT_ASSIGNED_CONTEXT((#9814,#9816,#9817))
REPRESENTATION_CONTEXT('','3D')
);
#9801=(
GEOMETRIC_REPRESENTATION_CONTEXT(3)
GLOBAL_UNCERTAINTY_ASSIGNED_CONTEXT((#9765))
GLOBAL_UNIT_ASSIGNED_CONTEXT((#9814,#9816,#9817))
REPRESENTATION_CONTEXT('','3D')
);
#9802=(
GEOMETRIC_REPRESENTATION_CONTEXT(3)
GLOBAL_UNCERTAINTY_ASSIGNED_CONTEXT((#9766))
GLOBAL_UNIT_ASSIGNED_CONTEXT((#9814,#9816,#9817))
REPRESENTATION_CONTEXT('','3D')
);
#9803=(
GEOMETRIC_REPRESENTATION_CONTEXT(3)
GLOBAL_UNCERTAINTY_ASSIGNED_CONTEXT((#9767))
GLOBAL_UNIT_ASSIGNED_CONTEXT((#9814,#9816,#9817))
REPRESENTATION_CONTEXT('','3D')
);
#9804=(
GEOMETRIC_REPRESENTATION_CONTEXT(3)
GLOBAL_UNCERTAINTY_ASSIGNED_CONTEXT((#9768))
GLOBAL_UNIT_ASSIGNED_CONTEXT((#9814,#9816,#9817))
REPRESENTATION_CONTEXT('','3D')
);
#9805=(
GEOMETRIC_REPRESENTATION_CONTEXT(3)
GLOBAL_UNCERTAINTY_ASSIGNED_CONTEXT((#9769))
GLOBAL_UNIT_ASSIGNED_CONTEXT((#9814,#9816,#9817))
REPRESENTATION_CONTEXT('','3D')
);
#9806=(
GEOMETRIC_REPRESENTATION_CONTEXT(3)
GLOBAL_UNCERTAINTY_ASSIGNED_CONTEXT((#9770))
GLOBAL_UNIT_ASSIGNED_CONTEXT((#9814,#9816,#9817))
REPRESENTATION_CONTEXT('','3D')
);
#9807=(
GEOMETRIC_REPRESENTATION_CONTEXT(3)
GLOBAL_UNCERTAINTY_ASSIGNED_CONTEXT((#9771))
GLOBAL_UNIT_ASSIGNED_CONTEXT((#9814,#9816,#9817))
REPRESENTATION_CONTEXT('','3D')
);
#9808=(
GEOMETRIC_REPRESENTATION_CONTEXT(3)
GLOBAL_UNCERTAINTY_ASSIGNED_CONTEXT((#9772))
GLOBAL_UNIT_ASSIGNED_CONTEXT((#9814,#9816,#9817))
REPRESENTATION_CONTEXT('','3D')
);
#9809=(
GEOMETRIC_REPRESENTATION_CONTEXT(3)
GLOBAL_UNCERTAINTY_ASSIGNED_CONTEXT((#9773))
GLOBAL_UNIT_ASSIGNED_CONTEXT((#9814,#9816,#9817))
REPRESENTATION_CONTEXT('','3D')
);
#9810=(
GEOMETRIC_REPRESENTATION_CONTEXT(3)
GLOBAL_UNCERTAINTY_ASSIGNED_CONTEXT((#9774))
GLOBAL_UNIT_ASSIGNED_CONTEXT((#9814,#9816,#9817))
REPRESENTATION_CONTEXT('','3D')
);
#9811=(
GEOMETRIC_REPRESENTATION_CONTEXT(3)
GLOBAL_UNCERTAINTY_ASSIGNED_CONTEXT((#9775))
GLOBAL_UNIT_ASSIGNED_CONTEXT((#9814,#9816,#9817))
REPRESENTATION_CONTEXT('','3D')
);
#9812=(
GEOMETRIC_REPRESENTATION_CONTEXT(3)
GLOBAL_UNCERTAINTY_ASSIGNED_CONTEXT((#9776))
GLOBAL_UNIT_ASSIGNED_CONTEXT((#9814,#9816,#9817))
REPRESENTATION_CONTEXT('','3D')
);
#9813=(
GEOMETRIC_REPRESENTATION_CONTEXT(3)
GLOBAL_UNCERTAINTY_ASSIGNED_CONTEXT((#9777))
GLOBAL_UNIT_ASSIGNED_CONTEXT((#9814,#9816,#9817))
REPRESENTATION_CONTEXT('','3D')
);
#9814=(
LENGTH_UNIT()
NAMED_UNIT(*)
SI_UNIT(.CENTI.,.METRE.)
);
#9815=(
LENGTH_UNIT()
NAMED_UNIT(*)
SI_UNIT($,.METRE.)
);
#9816=(
NAMED_UNIT(*)
PLANE_ANGLE_UNIT()
SI_UNIT($,.RADIAN.)
);
#9817=(
NAMED_UNIT(*)
SI_UNIT($,.STERADIAN.)
SOLID_ANGLE_UNIT()
);
#9818=SHAPE_DEFINITION_REPRESENTATION(#9853,#9935);
#9819=SHAPE_DEFINITION_REPRESENTATION(#9854,#9936);
#9820=SHAPE_DEFINITION_REPRESENTATION(#9855,#9937);
#9821=SHAPE_DEFINITION_REPRESENTATION(#9856,#9938);
#9822=SHAPE_DEFINITION_REPRESENTATION(#9857,#9939);
#9823=SHAPE_DEFINITION_REPRESENTATION(#9858,#9940);
#9824=SHAPE_DEFINITION_REPRESENTATION(#9859,#9941);
#9825=SHAPE_DEFINITION_REPRESENTATION(#9860,#9942);
#9826=SHAPE_DEFINITION_REPRESENTATION(#9861,#9943);
#9827=SHAPE_DEFINITION_REPRESENTATION(#9862,#9944);
#9828=SHAPE_DEFINITION_REPRESENTATION(#9863,#9945);
#9829=SHAPE_DEFINITION_REPRESENTATION(#9864,#9946);
#9830=SHAPE_DEFINITION_REPRESENTATION(#9865,#9947);
#9831=SHAPE_DEFINITION_REPRESENTATION(#9866,#9948);
#9832=SHAPE_DEFINITION_REPRESENTATION(#9867,#9949);
#9833=SHAPE_DEFINITION_REPRESENTATION(#9868,#9950);
#9834=SHAPE_DEFINITION_REPRESENTATION(#9869,#9951);
#9835=SHAPE_DEFINITION_REPRESENTATION(#9870,#9952);
#9836=SHAPE_DEFINITION_REPRESENTATION(#9871,#9953);
#9837=SHAPE_DEFINITION_REPRESENTATION(#9872,#9954);
#9838=SHAPE_DEFINITION_REPRESENTATION(#9873,#9955);
#9839=SHAPE_DEFINITION_REPRESENTATION(#9874,#9956);
#9840=SHAPE_DEFINITION_REPRESENTATION(#9875,#9957);
#9841=SHAPE_DEFINITION_REPRESENTATION(#9876,#9958);
#9842=SHAPE_DEFINITION_REPRESENTATION(#9877,#9959);
#9843=SHAPE_DEFINITION_REPRESENTATION(#9878,#9960);
#9844=SHAPE_DEFINITION_REPRESENTATION(#9879,#9961);
#9845=SHAPE_DEFINITION_REPRESENTATION(#9885,#9962);
#9846=SHAPE_DEFINITION_REPRESENTATION(#9919,#9963);
#9847=SHAPE_DEFINITION_REPRESENTATION(#9920,#9964);
#9848=SHAPE_DEFINITION_REPRESENTATION(#9921,#9965);
#9849=SHAPE_DEFINITION_REPRESENTATION(#9922,#9966);
#9850=SHAPE_DEFINITION_REPRESENTATION(#9923,#9967);
#9851=SHAPE_DEFINITION_REPRESENTATION(#9924,#9968);
#9852=SHAPE_DEFINITION_REPRESENTATION(#9925,#9969);
#9853=PRODUCT_DEFINITION_SHAPE('',$,#9971);
#9854=PRODUCT_DEFINITION_SHAPE('',$,#9972);
#9855=PRODUCT_DEFINITION_SHAPE('',$,#9973);
#9856=PRODUCT_DEFINITION_SHAPE('',$,#9974);
#9857=PRODUCT_DEFINITION_SHAPE('',$,#9975);
#9858=PRODUCT_DEFINITION_SHAPE('',$,#9976);
#9859=PRODUCT_DEFINITION_SHAPE('',$,#9977);
#9860=PRODUCT_DEFINITION_SHAPE('',$,#9978);
#9861=PRODUCT_DEFINITION_SHAPE('',$,#9979);
#9862=PRODUCT_DEFINITION_SHAPE('',$,#9980);
#9863=PRODUCT_DEFINITION_SHAPE('',$,#9981);
#9864=PRODUCT_DEFINITION_SHAPE('',$,#9982);
#9865=PRODUCT_DEFINITION_SHAPE('',$,#9983);
#9866=PRODUCT_DEFINITION_SHAPE('',$,#9984);
#9867=PRODUCT_DEFINITION_SHAPE('',$,#9985);
#9868=PRODUCT_DEFINITION_SHAPE('',$,#9986);
#9869=PRODUCT_DEFINITION_SHAPE('',$,#9987);
#9870=PRODUCT_DEFINITION_SHAPE('',$,#9988);
#9871=PRODUCT_DEFINITION_SHAPE('',$,#9989);
#9872=PRODUCT_DEFINITION_SHAPE('',$,#9990);
#9873=PRODUCT_DEFINITION_SHAPE('',$,#9991);
#9874=PRODUCT_DEFINITION_SHAPE('',$,#9992);
#9875=PRODUCT_DEFINITION_SHAPE('',$,#9993);
#9876=PRODUCT_DEFINITION_SHAPE('',$,#9994);
#9877=PRODUCT_DEFINITION_SHAPE('',$,#9995);
#9878=PRODUCT_DEFINITION_SHAPE('',$,#9996);
#9879=PRODUCT_DEFINITION_SHAPE('',$,#9997);
#9880=PRODUCT_DEFINITION_SHAPE($,$,#152);
#9881=PRODUCT_DEFINITION_SHAPE($,$,#153);
#9882=PRODUCT_DEFINITION_SHAPE($,$,#154);
#9883=PRODUCT_DEFINITION_SHAPE($,$,#155);
#9884=PRODUCT_DEFINITION_SHAPE($,$,#156);
#9885=PRODUCT_DEFINITION_SHAPE('',$,#9998);
#9886=PRODUCT_DEFINITION_SHAPE($,$,#157);
#9887=PRODUCT_DEFINITION_SHAPE($,$,#158);
#9888=PRODUCT_DEFINITION_SHAPE($,$,#159);
#9889=PRODUCT_DEFINITION_SHAPE($,$,#160);
#9890=PRODUCT_DEFINITION_SHAPE($,$,#161);
#9891=PRODUCT_DEFINITION_SHAPE($,$,#162);
#9892=PRODUCT_DEFINITION_SHAPE($,$,#163);
#9893=PRODUCT_DEFINITION_SHAPE($,$,#164);
#9894=PRODUCT_DEFINITION_SHAPE($,$,#165);
#9895=PRODUCT_DEFINITION_SHAPE($,$,#166);
#9896=PRODUCT_DEFINITION_SHAPE($,$,#167);
#9897=PRODUCT_DEFINITION_SHAPE($,$,#168);
#9898=PRODUCT_DEFINITION_SHAPE($,$,#169);
#9899=PRODUCT_DEFINITION_SHAPE($,$,#170);
#9900=PRODUCT_DEFINITION_SHAPE($,$,#171);
#9901=PRODUCT_DEFINITION_SHAPE($,$,#172);
#9902=PRODUCT_DEFINITION_SHAPE($,$,#173);
#9903=PRODUCT_DEFINITION_SHAPE($,$,#174);
#9904=PRODUCT_DEFINITION_SHAPE($,$,#175);
#9905=PRODUCT_DEFINITION_SHAPE($,$,#176);
#9906=PRODUCT_DEFINITION_SHAPE($,$,#177);
#9907=PRODUCT_DEFINITION_SHAPE($,$,#178);
#9908=PRODUCT_DEFINITION_SHAPE($,$,#179);
#9909=PRODUCT_DEFINITION_SHAPE($,$,#180);
#9910=PRODUCT_DEFINITION_SHAPE($,$,#181);
#9911=PRODUCT_DEFINITION_SHAPE($,$,#182);
#9912=PRODUCT_DEFINITION_SHAPE($,$,#183);
#9913=PRODUCT_DEFINITION_SHAPE($,$,#184);
#9914=PRODUCT_DEFINITION_SHAPE($,$,#185);
#9915=PRODUCT_DEFINITION_SHAPE($,$,#186);
#9916=PRODUCT_DEFINITION_SHAPE($,$,#187);
#9917=PRODUCT_DEFINITION_SHAPE($,$,#188);
#9918=PRODUCT_DEFINITION_SHAPE($,$,#189);
#9919=PRODUCT_DEFINITION_SHAPE('',$,#9999);
#9920=PRODUCT_DEFINITION_SHAPE('',$,#10000);
#9921=PRODUCT_DEFINITION_SHAPE('',$,#10001);
#9922=PRODUCT_DEFINITION_SHAPE('',$,#10002);
#9923=PRODUCT_DEFINITION_SHAPE('',$,#10003);
#9924=PRODUCT_DEFINITION_SHAPE('',$,#10004);
#9925=PRODUCT_DEFINITION_SHAPE('',$,#10005);
#9926=PRODUCT_DEFINITION_SHAPE($,$,#190);
#9927=PRODUCT_DEFINITION_SHAPE($,$,#191);
#9928=PRODUCT_DEFINITION_SHAPE($,$,#192);
#9929=PRODUCT_DEFINITION_SHAPE($,$,#193);
#9930=PRODUCT_DEFINITION_SHAPE($,$,#194);
#9931=PRODUCT_DEFINITION_SHAPE($,$,#195);
#9932=PRODUCT_DEFINITION_SHAPE($,$,#196);
#9933=PRODUCT_DEFINITION_SHAPE($,$,#197);
#9934=PRODUCT_DEFINITION_SHAPE($,$,#198);
#9935=SHAPE_REPRESENTATION('',(#5138,#5749,#5750),#9778);
#9936=SHAPE_REPRESENTATION('',(#5139,#5600,#5601,#5602,#5603,#5604,#5605,
#5606,#5607,#5608,#5609,#5610,#5611,#5612,#5613,#5614,#5615,#5616,#5617,
#5618,#5619,#5620,#5621,#5622,#5623,#5624,#5625,#5626,#5627,#5628,#5629,
#5630,#5631,#5632),#9779);
#9937=SHAPE_REPRESENTATION('',(#5140),#9780);
#9938=SHAPE_REPRESENTATION('',(#5159),#9781);
#9939=SHAPE_REPRESENTATION('',(#5166),#9782);
#9940=SHAPE_REPRESENTATION('',(#5173),#9783);
#9941=SHAPE_REPRESENTATION('',(#5198),#9784);
#9942=SHAPE_REPRESENTATION('',(#5217),#9785);
#9943=SHAPE_REPRESENTATION('',(#5242),#9786);
#9944=SHAPE_REPRESENTATION('',(#5278),#9787);
#9945=SHAPE_REPRESENTATION('',(#5303),#9788);
#9946=SHAPE_REPRESENTATION('',(#5339),#9789);
#9947=SHAPE_REPRESENTATION('',(#5355),#9790);
#9948=SHAPE_REPRESENTATION('',(#5358),#9791);
#9949=SHAPE_REPRESENTATION('',(#5368),#9792);
#9950=SHAPE_REPRESENTATION('',(#5381),#9793);
#9951=SHAPE_REPRESENTATION('',(#5390),#9794);
#9952=SHAPE_REPRESENTATION('',(#5395),#9795);
#9953=SHAPE_REPRESENTATION('',(#5402),#9796);
#9954=SHAPE_REPRESENTATION('',(#5409),#9797);
#9955=SHAPE_REPRESENTATION('',(#5418),#9798);
#9956=SHAPE_REPRESENTATION('',(#5442,#5571,#5572,#5573,#5574,#5575),#9799);
#9957=SHAPE_REPRESENTATION('',(#5443),#9800);
#9958=SHAPE_REPRESENTATION('',(#5463),#9801);
#9959=SHAPE_REPRESENTATION('',(#5483),#9802);
#9960=SHAPE_REPRESENTATION('',(#5500),#9803);
#9961=SHAPE_REPRESENTATION('',(#5554),#9804);
#9962=SHAPE_REPRESENTATION('',(#5576),#9805);
#9963=SHAPE_REPRESENTATION('',(#5633,#5742,#5743,#5744,#5745,#5746,#5747,
#5748),#9806);
#9964=SHAPE_REPRESENTATION('',(#5634),#9807);
#9965=SHAPE_REPRESENTATION('',(#5680),#9808);
#9966=SHAPE_REPRESENTATION('',(#5689),#9809);
#9967=SHAPE_REPRESENTATION('',(#5698),#9810);
#9968=SHAPE_REPRESENTATION('',(#5707),#9811);
#9969=SHAPE_REPRESENTATION('',(#5716),#9812);
#9970=PRODUCT_DEFINITION_CONTEXT('part definition',#10077,'design');
#9971=PRODUCT_DEFINITION('PAT-029',
'PAT-029',#10006,#9970);
#9972=PRODUCT_DEFINITION('Fixed leaf and test stand',
'Fixed leaf and test stand',#10007,#9970);
#9973=PRODUCT_DEFINITION('Base','Base',#10008,#9970);
#9974=PRODUCT_DEFINITION('Foot strip','Foot strip',#10009,#9970);
#9975=PRODUCT_DEFINITION('Foot strip (1)','Foot strip (1)',#10010,#9970);
#9976=PRODUCT_DEFINITION('Hinge post','Hinge post',#10011,#9970);
#9977=PRODUCT_DEFINITION('Fixed leaf','Fixed leaf',#10012,#9970);
#9978=PRODUCT_DEFINITION('Lower bearing carrier',
'Lower bearing carrier',#10013,#9970);
#9979=PRODUCT_DEFINITION('Bearing retaining cap',
'Bearing retaining cap',#10014,#9970);
#9980=PRODUCT_DEFINITION('Upper bearing carrier',
'Upper bearing carrier',#10015,#9970);
#9981=PRODUCT_DEFINITION('Bearing retaining cap (1)',
'Bearing retaining cap (1)',#10016,#9970);
#9982=PRODUCT_DEFINITION('Detent barrel','Detent barrel',#10017,#9970);
#9983=PRODUCT_DEFINITION('Detent ball','Detent ball',#10018,#9970);
#9984=PRODUCT_DEFINITION('Retract rod','Retract rod',#10019,#9970);
#9985=PRODUCT_DEFINITION('Rear spring plug','Rear spring plug',#10020,#9970);
#9986=PRODUCT_DEFINITION('Detent release knob','Detent release knob',#10021,
#9970);
#9987=PRODUCT_DEFINITION('Detent spring','Detent spring',#10022,#9970);
#9988=PRODUCT_DEFINITION('Open stop pedestal','Open stop pedestal',#10023,
#9970);
#9989=PRODUCT_DEFINITION('Stop bumper','Stop bumper',#10024,#9970);
#9990=PRODUCT_DEFINITION('Flat Washer - M6','Flat Washer - M6',#10025,#9970);
#9991=PRODUCT_DEFINITION('M6x18 mounting screw','M6x18 mounting screw',
#10026,#9970);
#9992=PRODUCT_DEFINITION('Sealed Ball Bearing - 10 x 30 x 9 mm',
'Sealed Ball Bearing - 10 x 30 x 9 mm',#10027,#9970);
#9993=PRODUCT_DEFINITION('Inner ring','Inner ring',#10028,#9970);
#9994=PRODUCT_DEFINITION('Outer ring','Outer ring',#10029,#9970);
#9995=PRODUCT_DEFINITION('Balls','Balls',#10030,#9970);
#9996=PRODUCT_DEFINITION('Cage','Cage',#10031,#9970);
#9997=PRODUCT_DEFINITION('Seals 2RS','Seals 2RS',#10032,#9970);
#9998=PRODUCT_DEFINITION('M4x10 Cap Screw','M4x10 Cap Screw',#10033,#9970);
#9999=PRODUCT_DEFINITION('Rotating leaf and hinge pin',
'Rotating leaf and hinge pin',#10034,#9970);
#10000=PRODUCT_DEFINITION('Moving leaf and hinge pin',
'Moving leaf and hinge pin',#10035,#9970);
#10001=PRODUCT_DEFINITION('Inner race spacer','Inner race spacer',#10036,
#9970);
#10002=PRODUCT_DEFINITION('Inner race spacer (1)','Inner race spacer (1)',
#10037,#9970);
#10003=PRODUCT_DEFINITION('Pin end keeper','Pin end keeper',#10038,#9970);
#10004=PRODUCT_DEFINITION('Pin end keeper (1)','Pin end keeper (1)',#10039,
#9970);
#10005=PRODUCT_DEFINITION('Cap Screw - M4x16','Cap Screw - M4x16',#10040,
#9970);
#10006=PRODUCT_DEFINITION_FORMATION('',$,#10079);
#10007=PRODUCT_DEFINITION_FORMATION('',$,#10080);
#10008=PRODUCT_DEFINITION_FORMATION('',$,#10081);
#10009=PRODUCT_DEFINITION_FORMATION('',$,#10082);
#10010=PRODUCT_DEFINITION_FORMATION('',$,#10083);
#10011=PRODUCT_DEFINITION_FORMATION('',$,#10084);
#10012=PRODUCT_DEFINITION_FORMATION('',$,#10085);
#10013=PRODUCT_DEFINITION_FORMATION('',$,#10086);
#10014=PRODUCT_DEFINITION_FORMATION('',$,#10087);
#10015=PRODUCT_DEFINITION_FORMATION('',$,#10088);
#10016=PRODUCT_DEFINITION_FORMATION('',$,#10089);
#10017=PRODUCT_DEFINITION_FORMATION('',$,#10090);
#10018=PRODUCT_DEFINITION_FORMATION('',$,#10091);
#10019=PRODUCT_DEFINITION_FORMATION('',$,#10092);
#10020=PRODUCT_DEFINITION_FORMATION('',$,#10093);
#10021=PRODUCT_DEFINITION_FORMATION('',$,#10094);
#10022=PRODUCT_DEFINITION_FORMATION('',$,#10095);
#10023=PRODUCT_DEFINITION_FORMATION('',$,#10096);
#10024=PRODUCT_DEFINITION_FORMATION('',$,#10097);
#10025=PRODUCT_DEFINITION_FORMATION('',$,#10098);
#10026=PRODUCT_DEFINITION_FORMATION('',$,#10099);
#10027=PRODUCT_DEFINITION_FORMATION('',$,#10100);
#10028=PRODUCT_DEFINITION_FORMATION('',$,#10101);
#10029=PRODUCT_DEFINITION_FORMATION('',$,#10102);
#10030=PRODUCT_DEFINITION_FORMATION('',$,#10103);
#10031=PRODUCT_DEFINITION_FORMATION('',$,#10104);
#10032=PRODUCT_DEFINITION_FORMATION('',$,#10105);
#10033=PRODUCT_DEFINITION_FORMATION('',$,#10106);
#10034=PRODUCT_DEFINITION_FORMATION('',$,#10107);
#10035=PRODUCT_DEFINITION_FORMATION('',$,#10108);
#10036=PRODUCT_DEFINITION_FORMATION('',$,#10109);
#10037=PRODUCT_DEFINITION_FORMATION('',$,#10110);
#10038=PRODUCT_DEFINITION_FORMATION('',$,#10111);
#10039=PRODUCT_DEFINITION_FORMATION('',$,#10112);
#10040=PRODUCT_DEFINITION_FORMATION('',$,#10113);
#10041=PRODUCT_RELATED_PRODUCT_CATEGORY('PAT-029','PAT-029',(#10079));
#10042=PRODUCT_RELATED_PRODUCT_CATEGORY('Fixed leaf and test stand',
'Fixed leaf and test stand',(#10080));
#10043=PRODUCT_RELATED_PRODUCT_CATEGORY('Base','Base',(#10081));
#10044=PRODUCT_RELATED_PRODUCT_CATEGORY('Foot strip','Foot strip',(#10082));
#10045=PRODUCT_RELATED_PRODUCT_CATEGORY('Foot strip (1)',
'Foot strip (1)',(#10083));
#10046=PRODUCT_RELATED_PRODUCT_CATEGORY('Hinge post','Hinge post',(#10084));
#10047=PRODUCT_RELATED_PRODUCT_CATEGORY('Fixed leaf','Fixed leaf',(#10085));
#10048=PRODUCT_RELATED_PRODUCT_CATEGORY('Lower bearing carrier',
'Lower bearing carrier',(#10086));
#10049=PRODUCT_RELATED_PRODUCT_CATEGORY('Bearing retaining cap',
'Bearing retaining cap',(#10087));
#10050=PRODUCT_RELATED_PRODUCT_CATEGORY('Upper bearing carrier',
'Upper bearing carrier',(#10088));
#10051=PRODUCT_RELATED_PRODUCT_CATEGORY('Bearing retaining cap (1)',
'Bearing retaining cap (1)',(#10089));
#10052=PRODUCT_RELATED_PRODUCT_CATEGORY('Detent barrel','Detent barrel',
(#10090));
#10053=PRODUCT_RELATED_PRODUCT_CATEGORY('Detent ball','Detent ball',(#10091));
#10054=PRODUCT_RELATED_PRODUCT_CATEGORY('Retract rod','Retract rod',(#10092));
#10055=PRODUCT_RELATED_PRODUCT_CATEGORY('Rear spring plug',
'Rear spring plug',(#10093));
#10056=PRODUCT_RELATED_PRODUCT_CATEGORY('Detent release knob',
'Detent release knob',(#10094));
#10057=PRODUCT_RELATED_PRODUCT_CATEGORY('Detent spring','Detent spring',
(#10095));
#10058=PRODUCT_RELATED_PRODUCT_CATEGORY('Open stop pedestal',
'Open stop pedestal',(#10096));
#10059=PRODUCT_RELATED_PRODUCT_CATEGORY('Stop bumper','Stop bumper',(#10097));
#10060=PRODUCT_RELATED_PRODUCT_CATEGORY('Flat Washer - M6',
'Flat Washer - M6',(#10098));
#10061=PRODUCT_RELATED_PRODUCT_CATEGORY('M6x18 mounting screw',
'M6x18 mounting screw',(#10099));
#10062=PRODUCT_RELATED_PRODUCT_CATEGORY(
'Sealed Ball Bearing - 10 x 30 x 9 mm',
'Sealed Ball Bearing - 10 x 30 x 9 mm',(#10100));
#10063=PRODUCT_RELATED_PRODUCT_CATEGORY('Inner ring','Inner ring',(#10101));
#10064=PRODUCT_RELATED_PRODUCT_CATEGORY('Outer ring','Outer ring',(#10102));
#10065=PRODUCT_RELATED_PRODUCT_CATEGORY('Balls','Balls',(#10103));
#10066=PRODUCT_RELATED_PRODUCT_CATEGORY('Cage','Cage',(#10104));
#10067=PRODUCT_RELATED_PRODUCT_CATEGORY('Seals 2RS','Seals 2RS',(#10105));
#10068=PRODUCT_RELATED_PRODUCT_CATEGORY('M4x10 Cap Screw',
'M4x10 Cap Screw',(#10106));
#10069=PRODUCT_RELATED_PRODUCT_CATEGORY('Rotating leaf and hinge pin',
'Rotating leaf and hinge pin',(#10107));
#10070=PRODUCT_RELATED_PRODUCT_CATEGORY('Moving leaf and hinge pin',
'Moving leaf and hinge pin',(#10108));
#10071=PRODUCT_RELATED_PRODUCT_CATEGORY('Inner race spacer',
'Inner race spacer',(#10109));
#10072=PRODUCT_RELATED_PRODUCT_CATEGORY('Inner race spacer (1)',
'Inner race spacer (1)',(#10110));
#10073=PRODUCT_RELATED_PRODUCT_CATEGORY('Pin end keeper',
'Pin end keeper',(#10111));
#10074=PRODUCT_RELATED_PRODUCT_CATEGORY('Pin end keeper (1)',
'Pin end keeper (1)',(#10112));
#10075=PRODUCT_RELATED_PRODUCT_CATEGORY('Cap Screw - M4x16',
'Cap Screw - M4x16',(#10113));
#10076=APPLICATION_PROTOCOL_DEFINITION('international standard',
'automotive_design',2009,#10077);
#10077=APPLICATION_CONTEXT(
'Core Data for Automotive Mechanical Design Process');
#10078=PRODUCT_CONTEXT('part definition',#10077,'mechanical');
#10079=PRODUCT('PAT-029','PAT-029',
'PAT-029',(#10078));
#10080=PRODUCT('Fixed leaf and test stand','Fixed leaf and test stand',
'Fixed leaf and test stand',(#10078));
#10081=PRODUCT('Base','Base','Base',(#10078));
#10082=PRODUCT('Foot strip','Foot strip','Foot strip',(#10078));
#10083=PRODUCT('Foot strip (1)','Foot strip (1)','Foot strip (1)',(#10078));
#10084=PRODUCT('Hinge post','Hinge post','Hinge post',(#10078));
#10085=PRODUCT('Fixed leaf','Fixed leaf','Fixed leaf',(#10078));
#10086=PRODUCT('Lower bearing carrier','Lower bearing carrier',
'Lower bearing carrier',(#10078));
#10087=PRODUCT('Bearing retaining cap','Bearing retaining cap',
'Bearing retaining cap',(#10078));
#10088=PRODUCT('Upper bearing carrier','Upper bearing carrier',
'Upper bearing carrier',(#10078));
#10089=PRODUCT('Bearing retaining cap (1)','Bearing retaining cap (1)',
'Bearing retaining cap (1)',(#10078));
#10090=PRODUCT('Detent barrel','Detent barrel','Detent barrel',(#10078));
#10091=PRODUCT('Detent ball','Detent ball','Detent ball',(#10078));
#10092=PRODUCT('Retract rod','Retract rod','Retract rod',(#10078));
#10093=PRODUCT('Rear spring plug','Rear spring plug','Rear spring plug',
(#10078));
#10094=PRODUCT('Detent release knob','Detent release knob',
'Detent release knob',(#10078));
#10095=PRODUCT('Detent spring','Detent spring','Detent spring',(#10078));
#10096=PRODUCT('Open stop pedestal','Open stop pedestal',
'Open stop pedestal',(#10078));
#10097=PRODUCT('Stop bumper','Stop bumper','Stop bumper',(#10078));
#10098=PRODUCT('Flat Washer - M6','Flat Washer - M6','Flat Washer - M6',
(#10078));
#10099=PRODUCT('M6x18 mounting screw','M6x18 mounting screw',
'M6x18 mounting screw',(#10078));
#10100=PRODUCT('Sealed Ball Bearing - 10 x 30 x 9 mm',
'Sealed Ball Bearing - 10 x 30 x 9 mm',
'Sealed Ball Bearing - 10 x 30 x 9 mm',(#10078));
#10101=PRODUCT('Inner ring','Inner ring','Inner ring',(#10078));
#10102=PRODUCT('Outer ring','Outer ring','Outer ring',(#10078));
#10103=PRODUCT('Balls','Balls','Balls',(#10078));
#10104=PRODUCT('Cage','Cage','Cage',(#10078));
#10105=PRODUCT('Seals 2RS','Seals 2RS','Seals 2RS',(#10078));
#10106=PRODUCT('M4x10 Cap Screw','M4x10 Cap Screw','M4x10 Cap Screw',(#10078));
#10107=PRODUCT('Rotating leaf and hinge pin',
'Rotating leaf and hinge pin','Rotating leaf and hinge pin',(#10078));
#10108=PRODUCT('Moving leaf and hinge pin','Moving leaf and hinge pin',
'Moving leaf and hinge pin',(#10078));
#10109=PRODUCT('Inner race spacer','Inner race spacer',
'Inner race spacer',(#10078));
#10110=PRODUCT('Inner race spacer (1)','Inner race spacer (1)',
'Inner race spacer (1)',(#10078));
#10111=PRODUCT('Pin end keeper','Pin end keeper','Pin end keeper',(#10078));
#10112=PRODUCT('Pin end keeper (1)','Pin end keeper (1)','Pin end keeper (1)',
(#10078));
#10113=PRODUCT('Cap Screw - M4x16','Cap Screw - M4x16',
'Cap Screw - M4x16',(#10078));
#10114=PRESENTATION_STYLE_ASSIGNMENT((#10120));
#10115=PRESENTATION_STYLE_ASSIGNMENT((#10121));
#10116=PRESENTATION_STYLE_ASSIGNMENT((#10122));
#10117=PRESENTATION_STYLE_ASSIGNMENT((#10123));
#10118=PRESENTATION_STYLE_ASSIGNMENT((#10124));
#10119=PRESENTATION_STYLE_ASSIGNMENT((#10125));
#10120=SURFACE_STYLE_USAGE(.BOTH.,#10126);
#10121=SURFACE_STYLE_USAGE(.BOTH.,#10127);
#10122=SURFACE_STYLE_USAGE(.BOTH.,#10128);
#10123=SURFACE_STYLE_USAGE(.BOTH.,#10129);
#10124=SURFACE_STYLE_USAGE(.BOTH.,#10130);
#10125=SURFACE_STYLE_USAGE(.BOTH.,#10131);
#10126=SURFACE_SIDE_STYLE('',(#10132));
#10127=SURFACE_SIDE_STYLE('',(#10133));
#10128=SURFACE_SIDE_STYLE('',(#10134));
#10129=SURFACE_SIDE_STYLE('',(#10135));
#10130=SURFACE_SIDE_STYLE('',(#10136));
#10131=SURFACE_SIDE_STYLE('',(#10137));
#10132=SURFACE_STYLE_FILL_AREA(#10138);
#10133=SURFACE_STYLE_FILL_AREA(#10139);
#10134=SURFACE_STYLE_FILL_AREA(#10140);
#10135=SURFACE_STYLE_FILL_AREA(#10141);
#10136=SURFACE_STYLE_FILL_AREA(#10142);
#10137=SURFACE_STYLE_FILL_AREA(#10143);
#10138=FILL_AREA_STYLE('Steel - Satin',(#10144));
#10139=FILL_AREA_STYLE('CAD Library Painted - Deep blue',(#10145));
#10140=FILL_AREA_STYLE('CAD Library Painted - Engineering blue',(#10146));
#10141=FILL_AREA_STYLE('CAD Library Painted - Steel gray',(#10147));
#10142=FILL_AREA_STYLE('CAD Library Painted - Graphite',(#10148));
#10143=FILL_AREA_STYLE('CAD Library Painted - Light blue',(#10149));
#10144=FILL_AREA_STYLE_COLOUR('Steel - Satin',#10150);
#10145=FILL_AREA_STYLE_COLOUR('CAD Library Painted - Deep blue',#10151);
#10146=FILL_AREA_STYLE_COLOUR('CAD Library Painted - Engineering blue',
#10152);
#10147=FILL_AREA_STYLE_COLOUR('CAD Library Painted - Steel gray',#10153);
#10148=FILL_AREA_STYLE_COLOUR('CAD Library Painted - Graphite',#10154);
#10149=FILL_AREA_STYLE_COLOUR('CAD Library Painted - Light blue',#10155);
#10150=COLOUR_RGB('Steel - Satin',0.627450980392157,0.627450980392157,0.627450980392157);
#10151=COLOUR_RGB('CAD Library Painted - Deep blue',0.0784313725490196,
0.203921568627451,0.349019607843137);
#10152=COLOUR_RGB('CAD Library Painted - Engineering blue',0.12156862745098,
0.356862745098039,0.6);
#10153=COLOUR_RGB('CAD Library Painted - Steel gray',0.592156862745098,
0.631372549019608,0.67843137254902);
#10154=COLOUR_RGB('CAD Library Painted - Graphite',0.168627450980392,0.192156862745098,
0.231372549019608);
#10155=COLOUR_RGB('CAD Library Painted - Light blue',0.286274509803922,
0.552941176470588,0.780392156862745);
#10156=COLOUR_RGB('Dark Blue',0.08,0.2,0.34);
#10157=FILL_AREA_STYLE_COLOUR('',#10156);
#10158=FILL_AREA_STYLE('',(#10157));
#10159=SURFACE_STYLE_FILL_AREA(#10158);
#10160=SURFACE_SIDE_STYLE('',(#10159));
#10161=SURFACE_STYLE_USAGE(.BOTH.,#10160);
#10162=PRESENTATION_STYLE_ASSIGNMENT((#10161));
#10163=COLOUR_RGB('Light Blue',0.38,0.62,0.78);
#10164=FILL_AREA_STYLE_COLOUR('',#10163);
#10165=FILL_AREA_STYLE('',(#10164));
#10166=SURFACE_STYLE_FILL_AREA(#10165);
#10167=SURFACE_SIDE_STYLE('',(#10166));
#10168=SURFACE_STYLE_USAGE(.BOTH.,#10167);
#10169=PRESENTATION_STYLE_ASSIGNMENT((#10168));
#10170=COLOUR_RGB('Sky Blue',0.24,0.69,0.87);
#10171=FILL_AREA_STYLE_COLOUR('',#10170);
#10172=FILL_AREA_STYLE('',(#10171));
#10173=SURFACE_STYLE_FILL_AREA(#10172);
#10174=SURFACE_SIDE_STYLE('',(#10173));
#10175=SURFACE_STYLE_USAGE(.BOTH.,#10174);
#10176=PRESENTATION_STYLE_ASSIGNMENT((#10175));
#10177=COLOUR_RGB('Grey',0.48,0.52,0.57);
#10178=FILL_AREA_STYLE_COLOUR('',#10177);
#10179=FILL_AREA_STYLE('',(#10178));
#10180=SURFACE_STYLE_FILL_AREA(#10179);
#10181=SURFACE_SIDE_STYLE('',(#10180));
#10182=SURFACE_STYLE_USAGE(.BOTH.,#10181);
#10183=PRESENTATION_STYLE_ASSIGNMENT((#10182));
#10184=COLOUR_RGB('Black',0.12,0.14,0.17);
#10185=FILL_AREA_STYLE_COLOUR('',#10184);
#10186=FILL_AREA_STYLE('',(#10185));
#10187=SURFACE_STYLE_FILL_AREA(#10186);
#10188=SURFACE_SIDE_STYLE('',(#10187));
#10189=SURFACE_STYLE_USAGE(.BOTH.,#10188);
#10190=PRESENTATION_STYLE_ASSIGNMENT((#10189));
#10191=COLOUR_RGB('Off White',0.89,0.88,0.83);
#10192=FILL_AREA_STYLE_COLOUR('',#10191);
#10193=FILL_AREA_STYLE('',(#10192));
#10194=SURFACE_STYLE_FILL_AREA(#10193);
#10195=SURFACE_SIDE_STYLE('',(#10194));
#10196=SURFACE_STYLE_USAGE(.BOTH.,#10195);
#10197=PRESENTATION_STYLE_ASSIGNMENT((#10196));
ENDSEC;
END-ISO-10303-21;
